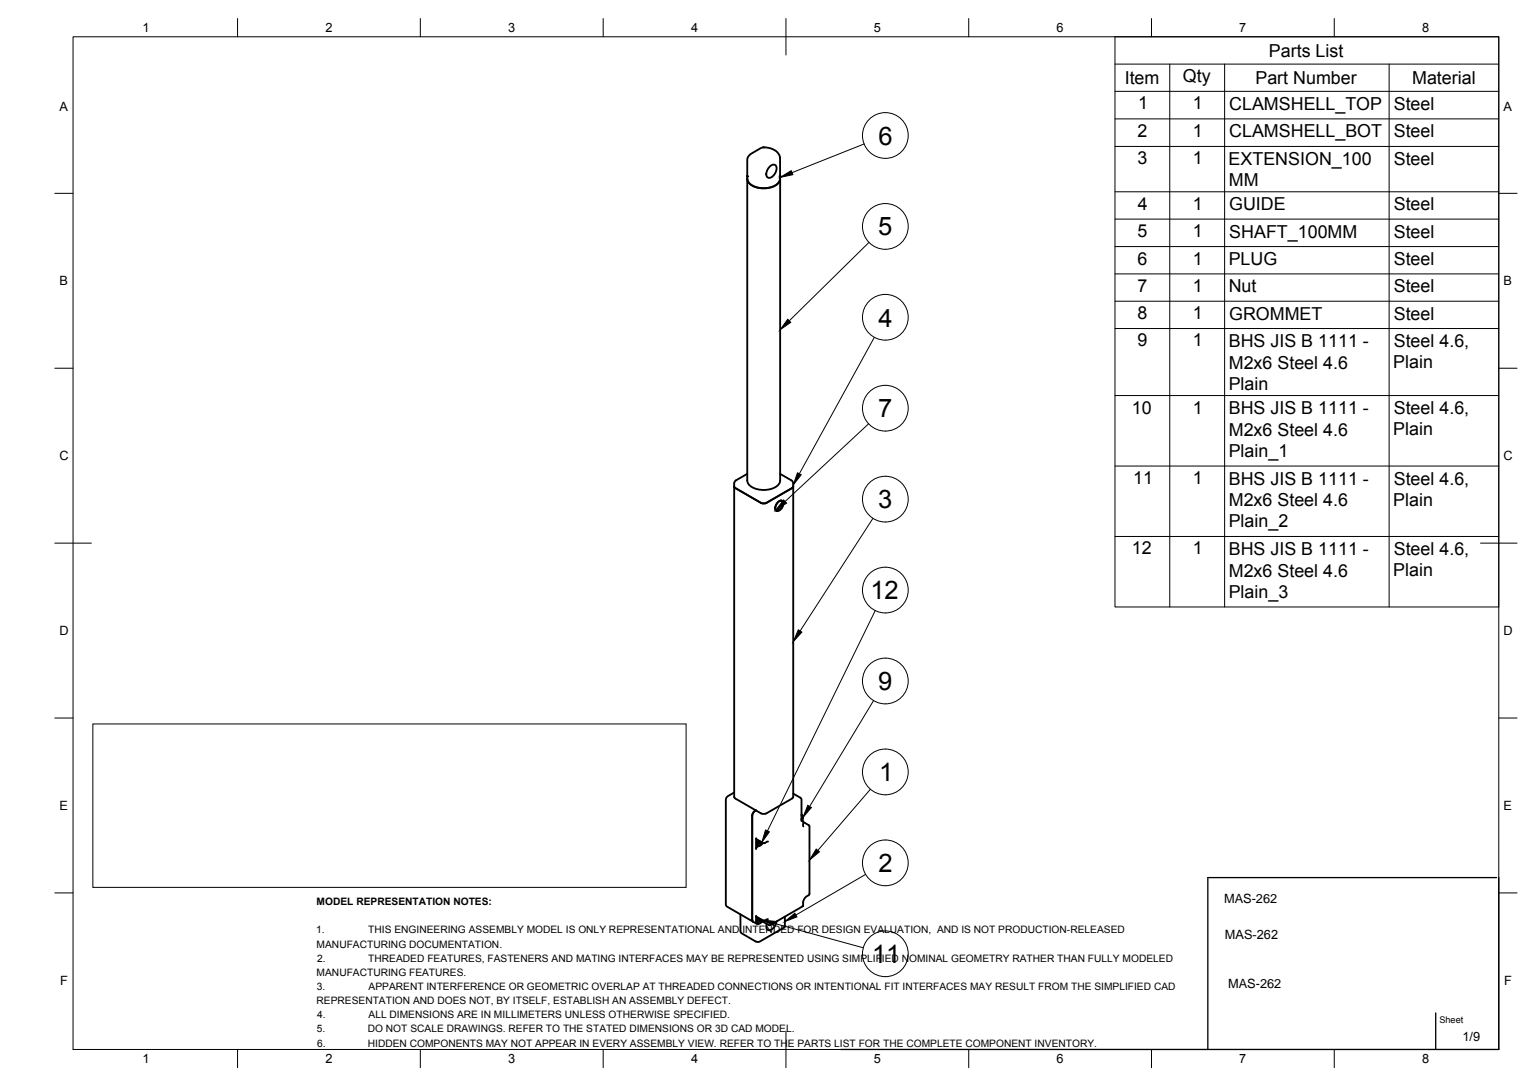
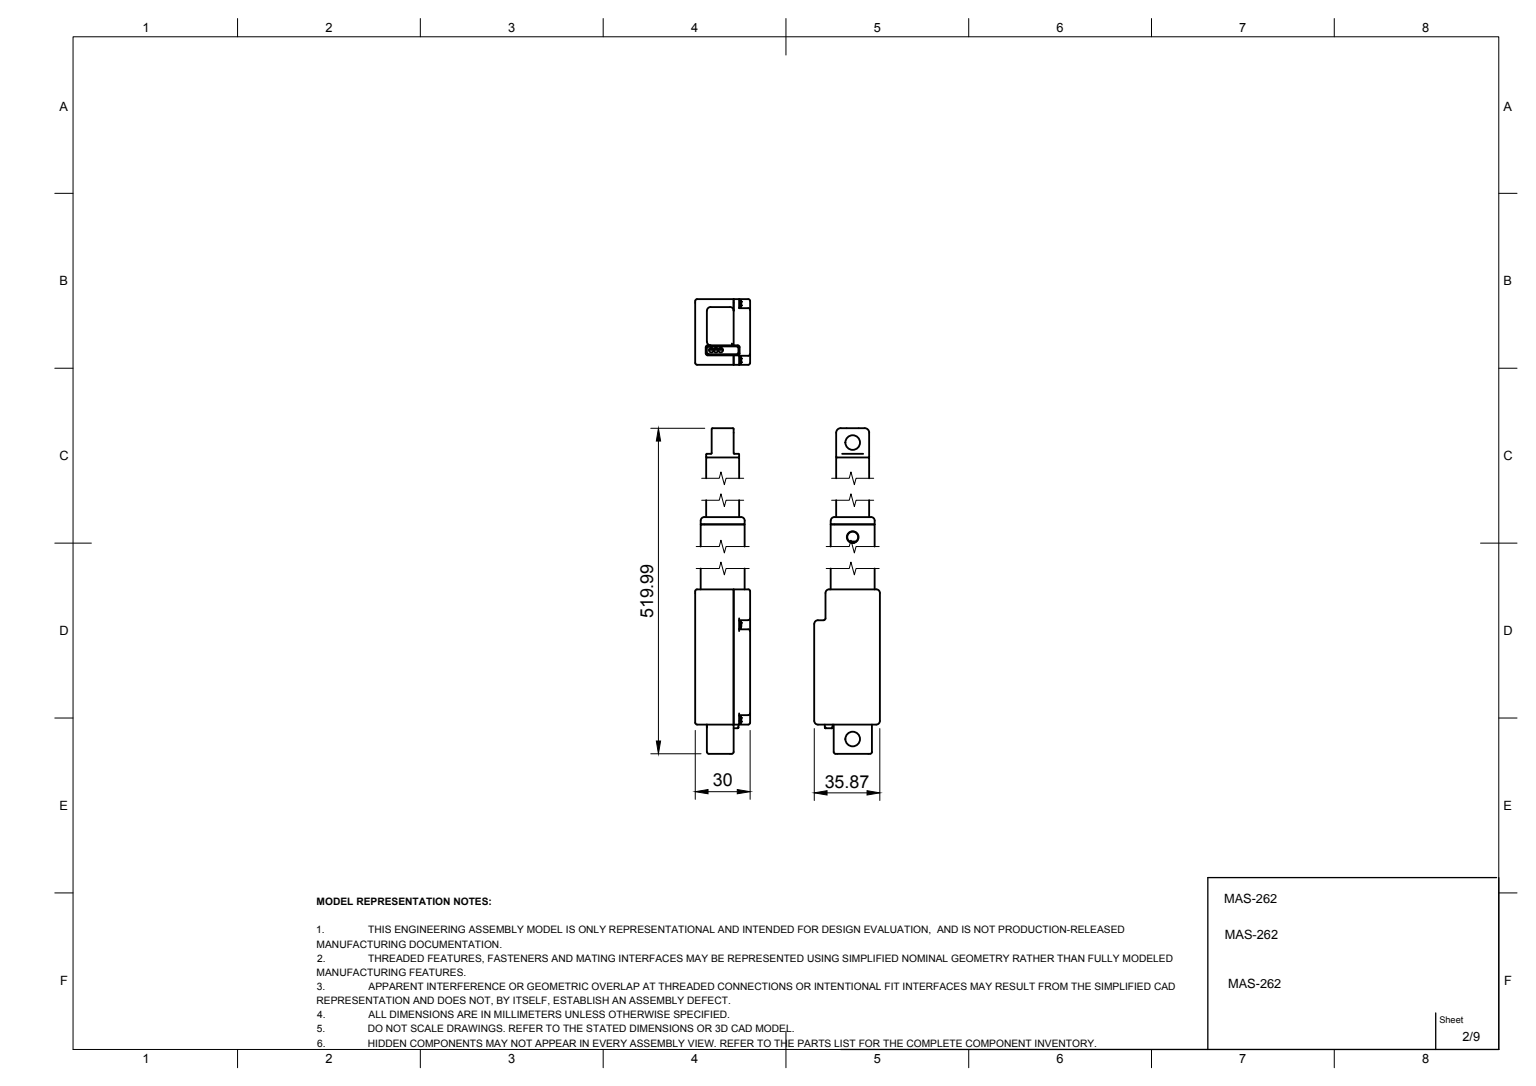
ISO-10303-21;
HEADER;
/* Generated by software containing ST-Developer
 * from STEP Tools, Inc. (www.steptools.com) 
 */

FILE_DESCRIPTION(
/* description */ (''),
/* implementation_level */ '2;1');

FILE_NAME(
/* name */ 'MAS-262',
/* time_stamp */ '2026-10-07T02:13:48+06:00',
/* author */ (''),
/* organization */ (''),
/* preprocessor_version */ 'ST-DEVELOPER v20.2',
/* originating_system */ 'Autodesk Translation Framework v15.15.0.0',
/* authorisation */ '');

FILE_SCHEMA (('AUTOMOTIVE_DESIGN { 1 0 10303 214 3 1 1 }'));
ENDSEC;

DATA;
#10=MECHANICAL_DESIGN_GEOMETRIC_PRESENTATION_REPRESENTATION('',(#114,#115,
#116,#117,#118,#119,#120,#121,#122,#123,#124,#125),#17042);
#11=ITEM_DEFINED_TRANSFORMATION($,$,#8261,#9239);
#12=ITEM_DEFINED_TRANSFORMATION($,$,#8462,#9240);
#13=ITEM_DEFINED_TRANSFORMATION($,$,#8601,#9241);
#14=ITEM_DEFINED_TRANSFORMATION($,$,#8648,#9242);
#15=ITEM_DEFINED_TRANSFORMATION($,$,#8826,#9243);
#16=ITEM_DEFINED_TRANSFORMATION($,$,#8839,#9244);
#17=ITEM_DEFINED_TRANSFORMATION($,$,#8908,#9245);
#18=ITEM_DEFINED_TRANSFORMATION($,$,#8935,#9246);
#19=ITEM_DEFINED_TRANSFORMATION($,$,#8995,#9247);
#20=ITEM_DEFINED_TRANSFORMATION($,$,#9056,#9248);
#21=ITEM_DEFINED_TRANSFORMATION($,$,#9117,#9249);
#22=ITEM_DEFINED_TRANSFORMATION($,$,#9178,#9250);
#23=(
REPRESENTATION_RELATIONSHIP($,$,#17086,#17085)
REPRESENTATION_RELATIONSHIP_WITH_TRANSFORMATION(#11)
SHAPE_REPRESENTATION_RELATIONSHIP()
);
#24=(
REPRESENTATION_RELATIONSHIP($,$,#17087,#17085)
REPRESENTATION_RELATIONSHIP_WITH_TRANSFORMATION(#12)
SHAPE_REPRESENTATION_RELATIONSHIP()
);
#25=(
REPRESENTATION_RELATIONSHIP($,$,#17088,#17085)
REPRESENTATION_RELATIONSHIP_WITH_TRANSFORMATION(#13)
SHAPE_REPRESENTATION_RELATIONSHIP()
);
#26=(
REPRESENTATION_RELATIONSHIP($,$,#17089,#17085)
REPRESENTATION_RELATIONSHIP_WITH_TRANSFORMATION(#14)
SHAPE_REPRESENTATION_RELATIONSHIP()
);
#27=(
REPRESENTATION_RELATIONSHIP($,$,#17090,#17085)
REPRESENTATION_RELATIONSHIP_WITH_TRANSFORMATION(#15)
SHAPE_REPRESENTATION_RELATIONSHIP()
);
#28=(
REPRESENTATION_RELATIONSHIP($,$,#17091,#17085)
REPRESENTATION_RELATIONSHIP_WITH_TRANSFORMATION(#16)
SHAPE_REPRESENTATION_RELATIONSHIP()
);
#29=(
REPRESENTATION_RELATIONSHIP($,$,#17092,#17085)
REPRESENTATION_RELATIONSHIP_WITH_TRANSFORMATION(#17)
SHAPE_REPRESENTATION_RELATIONSHIP()
);
#30=(
REPRESENTATION_RELATIONSHIP($,$,#17093,#17085)
REPRESENTATION_RELATIONSHIP_WITH_TRANSFORMATION(#18)
SHAPE_REPRESENTATION_RELATIONSHIP()
);
#31=(
REPRESENTATION_RELATIONSHIP($,$,#17094,#17085)
REPRESENTATION_RELATIONSHIP_WITH_TRANSFORMATION(#19)
SHAPE_REPRESENTATION_RELATIONSHIP()
);
#32=(
REPRESENTATION_RELATIONSHIP($,$,#17095,#17085)
REPRESENTATION_RELATIONSHIP_WITH_TRANSFORMATION(#20)
SHAPE_REPRESENTATION_RELATIONSHIP()
);
#33=(
REPRESENTATION_RELATIONSHIP($,$,#17096,#17085)
REPRESENTATION_RELATIONSHIP_WITH_TRANSFORMATION(#21)
SHAPE_REPRESENTATION_RELATIONSHIP()
);
#34=(
REPRESENTATION_RELATIONSHIP($,$,#17097,#17085)
REPRESENTATION_RELATIONSHIP_WITH_TRANSFORMATION(#22)
SHAPE_REPRESENTATION_RELATIONSHIP()
);
#35=CONTEXT_DEPENDENT_SHAPE_REPRESENTATION(#23,#17073);
#36=CONTEXT_DEPENDENT_SHAPE_REPRESENTATION(#24,#17074);
#37=CONTEXT_DEPENDENT_SHAPE_REPRESENTATION(#25,#17075);
#38=CONTEXT_DEPENDENT_SHAPE_REPRESENTATION(#26,#17076);
#39=CONTEXT_DEPENDENT_SHAPE_REPRESENTATION(#27,#17077);
#40=CONTEXT_DEPENDENT_SHAPE_REPRESENTATION(#28,#17078);
#41=CONTEXT_DEPENDENT_SHAPE_REPRESENTATION(#29,#17079);
#42=CONTEXT_DEPENDENT_SHAPE_REPRESENTATION(#30,#17080);
#43=CONTEXT_DEPENDENT_SHAPE_REPRESENTATION(#31,#17081);
#44=CONTEXT_DEPENDENT_SHAPE_REPRESENTATION(#32,#17082);
#45=CONTEXT_DEPENDENT_SHAPE_REPRESENTATION(#33,#17083);
#46=CONTEXT_DEPENDENT_SHAPE_REPRESENTATION(#34,#17084);
#47=NEXT_ASSEMBLY_USAGE_OCCURRENCE('CLAMSHELL_TOP:1','CLAMSHELL_TOP:1',
'CLAMSHELL_TOP:1',#17099,#17100,'CLAMSHELL_TOP:1');
#48=NEXT_ASSEMBLY_USAGE_OCCURRENCE('CLAMSHELL_BOT:1','CLAMSHELL_BOT:1',
'CLAMSHELL_BOT:1',#17099,#17101,'CLAMSHELL_BOT:1');
#49=NEXT_ASSEMBLY_USAGE_OCCURRENCE('EXTENSION_100MM:1',
'EXTENSION_100MM:1','EXTENSION_100MM:1',#17099,#17102,
'EXTENSION_100MM:1');
#50=NEXT_ASSEMBLY_USAGE_OCCURRENCE('GUIDE:1','GUIDE:1','GUIDE:1',#17099,
#17103,'GUIDE:1');
#51=NEXT_ASSEMBLY_USAGE_OCCURRENCE('SHAFT_100MM:1','SHAFT_100MM:1',
'SHAFT_100MM:1',#17099,#17104,'SHAFT_100MM:1');
#52=NEXT_ASSEMBLY_USAGE_OCCURRENCE('PLUG:1','PLUG:1','PLUG:1',#17099,#17105,
'PLUG:1');
#53=NEXT_ASSEMBLY_USAGE_OCCURRENCE('Nut:1','Nut:1','Nut:1',#17099,#17106,
'Nut:1');
#54=NEXT_ASSEMBLY_USAGE_OCCURRENCE('GROMMET:1','GROMMET:1','GROMMET:1',
#17099,#17107,'GROMMET:1');
#55=NEXT_ASSEMBLY_USAGE_OCCURRENCE(
'Binding Head Screw JIS B 1111 - M2x6 Steel 4.6 Plain v1:1',
'Binding Head Screw JIS B 1111 - M2x6 Steel 4.6 Plain v1:1',
'Binding Head Screw JIS B 1111 - M2x6 Steel 4.6 Plain v1:1',#17099,#17108,
'Binding Head Screw JIS B 1111 - M2x6 Steel 4.6 Plain v1:1');
#56=NEXT_ASSEMBLY_USAGE_OCCURRENCE(
'Binding Head Screw JIS B 1111 - M2x6 Steel 4.6 Plain v1 (2):1',
'Binding Head Screw JIS B 1111 - M2x6 Steel 4.6 Plain v1 (2):1',
'Binding Head Screw JIS B 1111 - M2x6 Steel 4.6 Plain v1 (2):1',#17099,
#17109,'Binding Head Screw JIS B 1111 - M2x6 Steel 4.6 Plain v1 (2):1');
#57=NEXT_ASSEMBLY_USAGE_OCCURRENCE(
'Binding Head Screw JIS B 1111 - M2x6 Steel 4.6 Plain v1 (3):1',
'Binding Head Screw JIS B 1111 - M2x6 Steel 4.6 Plain v1 (3):1',
'Binding Head Screw JIS B 1111 - M2x6 Steel 4.6 Plain v1 (3):1',#17099,
#17110,'Binding Head Screw JIS B 1111 - M2x6 Steel 4.6 Plain v1 (3):1');
#58=NEXT_ASSEMBLY_USAGE_OCCURRENCE(
'Binding Head Screw JIS B 1111 - M2x6 Steel 4.6 Plain v1 (1):1',
'Binding Head Screw JIS B 1111 - M2x6 Steel 4.6 Plain v1 (1):1',
'Binding Head Screw JIS B 1111 - M2x6 Steel 4.6 Plain v1 (1):1',#17099,
#17111,'Binding Head Screw JIS B 1111 - M2x6 Steel 4.6 Plain v1 (1):1');
#59=CONICAL_SURFACE('',#8827,7.5,0.785398163397441);
#60=CONICAL_SURFACE('',#8834,7.5,0.785398163397441);
#61=CONICAL_SURFACE('',#8902,5.5,0.785398163397441);
#62=CONICAL_SURFACE('',#9046,0.919615242270664,0.261799387799148);
#63=CONICAL_SURFACE('',#9055,2.11281731799709,0.0872664626099693);
#64=CONICAL_SURFACE('',#9107,0.919615242270664,0.261799387799148);
#65=CONICAL_SURFACE('',#9116,2.11281731799709,0.0872664626099693);
#66=CONICAL_SURFACE('',#9168,0.919615242270664,0.261799387799148);
#67=CONICAL_SURFACE('',#9177,2.11281731799709,0.0872664626099693);
#68=CONICAL_SURFACE('',#9229,0.919615242270664,0.261799387799148);
#69=CONICAL_SURFACE('',#9238,2.11281731799709,0.0872664626099693);
#70=B_SPLINE_SURFACE_WITH_KNOTS('',3,3,((#13032,#13033,#13034,#13035,#13036),
(#13037,#13038,#13039,#13040,#13041),(#13042,#13043,#13044,#13045,#13046),
(#13047,#13048,#13049,#13050,#13051),(#13052,#13053,#13054,#13055,#13056),
(#13057,#13058,#13059,#13060,#13061),(#13062,#13063,#13064,#13065,#13066)),
 .UNSPECIFIED.,.F.,.F.,.F.,(4,1,1,1,4),(4,1,4),(0.,0.285714285714286,0.571428571428571,
0.857142857142857,1.),(0.,0.020779022277979,0.0415580445559579),
 .UNSPECIFIED.);
#71=B_SPLINE_SURFACE_WITH_KNOTS('',3,3,((#13080,#13081,#13082,#13083,#13084,
#13085),(#13086,#13087,#13088,#13089,#13090,#13091),(#13092,#13093,#13094,
#13095,#13096,#13097),(#13098,#13099,#13100,#13101,#13102,#13103),(#13104,
#13105,#13106,#13107,#13108,#13109),(#13110,#13111,#13112,#13113,#13114,
#13115),(#13116,#13117,#13118,#13119,#13120,#13121)),.UNSPECIFIED.,.F.,
 .F.,.F.,(4,1,1,1,4),(4,1,1,4),(0.,0.285714285714286,0.571428571428571,
0.857142857142857,1.),(-0.417579612421967,-0.0596542303459957,0.178962691037985,
0.417579612421966),.UNSPECIFIED.);
#72=B_SPLINE_SURFACE_WITH_KNOTS('',3,3,((#13127,#13128,#13129,#13130,#13131),
(#13132,#13133,#13134,#13135,#13136),(#13137,#13138,#13139,#13140,#13141),
(#13142,#13143,#13144,#13145,#13146),(#13147,#13148,#13149,#13150,#13151),
(#13152,#13153,#13154,#13155,#13156),(#13157,#13158,#13159,#13160,#13161)),
 .UNSPECIFIED.,.F.,.F.,.F.,(4,1,1,1,4),(4,1,4),(0.,0.285714285714286,0.571428571428571,
0.857142857142857,1.),(0.,0.0207805027277528,0.0415610054555056),
 .UNSPECIFIED.);
#73=B_SPLINE_SURFACE_WITH_KNOTS('',3,3,((#13236,#13237,#13238,#13239,#13240),
(#13241,#13242,#13243,#13244,#13245),(#13246,#13247,#13248,#13249,#13250),
(#13251,#13252,#13253,#13254,#13255),(#13256,#13257,#13258,#13259,#13260),
(#13261,#13262,#13263,#13264,#13265),(#13266,#13267,#13268,#13269,#13270)),
 .UNSPECIFIED.,.F.,.F.,.F.,(4,1,1,1,4),(4,1,4),(0.,0.285714285714286,0.571428571428571,
0.857142857142857,1.),(0.,0.0207790222779789,0.0415580445559579),
 .UNSPECIFIED.);
#74=B_SPLINE_SURFACE_WITH_KNOTS('',3,3,((#13284,#13285,#13286,#13287,#13288,
#13289),(#13290,#13291,#13292,#13293,#13294,#13295),(#13296,#13297,#13298,
#13299,#13300,#13301),(#13302,#13303,#13304,#13305,#13306,#13307),(#13308,
#13309,#13310,#13311,#13312,#13313),(#13314,#13315,#13316,#13317,#13318,
#13319),(#13320,#13321,#13322,#13323,#13324,#13325)),.UNSPECIFIED.,.F.,
 .F.,.F.,(4,1,1,1,4),(4,1,1,4),(0.,0.285714285714286,0.571428571428571,
0.857142857142857,1.),(-0.417579612421968,-0.0596542303459959,0.178962691037985,
0.417579612421966),.UNSPECIFIED.);
#75=B_SPLINE_SURFACE_WITH_KNOTS('',3,3,((#13331,#13332,#13333,#13334,#13335),
(#13336,#13337,#13338,#13339,#13340),(#13341,#13342,#13343,#13344,#13345),
(#13346,#13347,#13348,#13349,#13350),(#13351,#13352,#13353,#13354,#13355),
(#13356,#13357,#13358,#13359,#13360),(#13361,#13362,#13363,#13364,#13365)),
 .UNSPECIFIED.,.F.,.F.,.F.,(4,1,1,1,4),(4,1,4),(0.,0.285714285714286,0.571428571428571,
0.857142857142857,1.),(0.,0.0207805027277526,0.0415610054555052),
 .UNSPECIFIED.);
#76=B_SPLINE_SURFACE_WITH_KNOTS('',3,3,((#13698,#13699,#13700,#13701,#13702,
#13703),(#13704,#13705,#13706,#13707,#13708,#13709),(#13710,#13711,#13712,
#13713,#13714,#13715),(#13716,#13717,#13718,#13719,#13720,#13721),(#13722,
#13723,#13724,#13725,#13726,#13727)),.UNSPECIFIED.,.F.,.F.,.F.,(4,1,4),
(4,1,1,4),(0.,0.5,1.),(0.,0.0435664957825988,0.0599039317010734,0.0762413676195479),
 .UNSPECIFIED.);
#77=B_SPLINE_SURFACE_WITH_KNOTS('',3,3,((#13746,#13747,#13748,#13749,#13750,
#13751),(#13752,#13753,#13754,#13755,#13756,#13757),(#13758,#13759,#13760,
#13761,#13762,#13763),(#13764,#13765,#13766,#13767,#13768,#13769),(#13770,
#13771,#13772,#13773,#13774,#13775)),.UNSPECIFIED.,.F.,.F.,.F.,(4,1,4),
(4,1,1,4),(0.,0.5,1.),(0.,0.0163372895861103,0.0326745791722206,0.0762406847351813),
 .UNSPECIFIED.);
#78=B_SPLINE_SURFACE_WITH_KNOTS('',3,3,((#13800,#13801,#13802,#13803,#13804,
#13805),(#13806,#13807,#13808,#13809,#13810,#13811),(#13812,#13813,#13814,
#13815,#13816,#13817),(#13818,#13819,#13820,#13821,#13822,#13823),(#13824,
#13825,#13826,#13827,#13828,#13829)),.UNSPECIFIED.,.F.,.F.,.F.,(4,1,4),
(4,1,1,4),(0.,0.5,1.),(3.96177645312185E-16,0.061147749085529,0.0917216236282934,
0.214017121799351),.UNSPECIFIED.);
#79=B_SPLINE_SURFACE_WITH_KNOTS('',3,3,((#13851,#13852,#13853,#13854,#13855,
#13856),(#13857,#13858,#13859,#13860,#13861,#13862),(#13863,#13864,#13865,
#13866,#13867,#13868),(#13869,#13870,#13871,#13872,#13873,#13874),(#13875,
#13876,#13877,#13878,#13879,#13880)),.UNSPECIFIED.,.F.,.F.,.F.,(4,1,4),
(4,1,1,4),(0.,0.5,1.),(2.01858731750029E-18,0.0917257862177262,0.152876310362877,
0.214026834508028),.UNSPECIFIED.);
#80=B_SPLINE_SURFACE_WITH_KNOTS('',3,3,((#13926,#13927,#13928,#13929,#13930,
#13931),(#13932,#13933,#13934,#13935,#13936,#13937),(#13938,#13939,#13940,
#13941,#13942,#13943),(#13944,#13945,#13946,#13947,#13948,#13949),(#13950,
#13951,#13952,#13953,#13954,#13955)),.UNSPECIFIED.,.F.,.F.,.F.,(4,1,4),
(4,1,1,4),(0.,0.5,1.),(0.,0.0163372896496662,0.0326745792993324,0.0762406850317755),
 .UNSPECIFIED.);
#81=B_SPLINE_SURFACE_WITH_KNOTS('',3,3,((#13974,#13975,#13976,#13977,#13978,
#13979),(#13980,#13981,#13982,#13983,#13984,#13985),(#13986,#13987,#13988,
#13989,#13990,#13991),(#13992,#13993,#13994,#13995,#13996,#13997),(#13998,
#13999,#14000,#14001,#14002,#14003)),.UNSPECIFIED.,.F.,.F.,.F.,(4,1,4),
(4,1,1,4),(0.,0.5,1.),(7.01665201425609E-18,0.0435664948259872,0.0599039303857324,
0.0762413659454776),.UNSPECIFIED.);
#82=B_SPLINE_SURFACE_WITH_KNOTS('',3,3,((#14027,#14028,#14029,#14030,#14031,
#14032),(#14033,#14034,#14035,#14036,#14037,#14038),(#14039,#14040,#14041,
#14042,#14043,#14044),(#14045,#14046,#14047,#14048,#14049,#14050),(#14051,
#14052,#14053,#14054,#14055,#14056)),.UNSPECIFIED.,.F.,.F.,.F.,(4,1,4),
(4,1,1,4),(0.,0.5,1.),(6.74145042959343E-15,0.0611477488274177,0.0917216232411232,
0.214017120895945),.UNSPECIFIED.);
#83=B_SPLINE_SURFACE_WITH_KNOTS('',3,3,((#14069,#14070,#14071,#14072,#14073,
#14074),(#14075,#14076,#14077,#14078,#14079,#14080),(#14081,#14082,#14083,
#14084,#14085,#14086),(#14087,#14088,#14089,#14090,#14091,#14092),(#14093,
#14094,#14095,#14096,#14097,#14098)),.UNSPECIFIED.,.F.,.F.,.F.,(4,1,4),
(4,1,1,4),(0.,0.5,1.),(0.,0.0917257862177262,0.152876310362877,0.214026834508028),
 .UNSPECIFIED.);
#84=B_SPLINE_SURFACE_WITH_KNOTS('',3,3,((#14832,#14833,#14834,#14835,#14836,
#14837,#14838,#14839,#14840,#14841,#14842,#14843,#14844,#14845,#14846,#14847,
#14848,#14849,#14850,#14851,#14852,#14853,#14854,#14855,#14856,#14857,#14858,
#14859,#14860,#14861,#14862,#14863,#14864,#14865,#14866,#14867,#14868,#14869,
#14870,#14871,#14872,#14873,#14874,#14875,#14876,#14877,#14878,#14879,#14880,
#14881,#14882,#14883,#14884,#14885,#14886,#14887,#14888,#14889,#14890,#14891,
#14892,#14893,#14894,#14895,#14896,#14897,#14898,#14899,#14900,#14901,#14902,
#14903,#14904,#14905,#14906,#14907,#14908,#14909,#14910),(#14911,#14912,
#14913,#14914,#14915,#14916,#14917,#14918,#14919,#14920,#14921,#14922,#14923,
#14924,#14925,#14926,#14927,#14928,#14929,#14930,#14931,#14932,#14933,#14934,
#14935,#14936,#14937,#14938,#14939,#14940,#14941,#14942,#14943,#14944,#14945,
#14946,#14947,#14948,#14949,#14950,#14951,#14952,#14953,#14954,#14955,#14956,
#14957,#14958,#14959,#14960,#14961,#14962,#14963,#14964,#14965,#14966,#14967,
#14968,#14969,#14970,#14971,#14972,#14973,#14974,#14975,#14976,#14977,#14978,
#14979,#14980,#14981,#14982,#14983,#14984,#14985,#14986,#14987,#14988,#14989),
(#14990,#14991,#14992,#14993,#14994,#14995,#14996,#14997,#14998,#14999,
#15000,#15001,#15002,#15003,#15004,#15005,#15006,#15007,#15008,#15009,#15010,
#15011,#15012,#15013,#15014,#15015,#15016,#15017,#15018,#15019,#15020,#15021,
#15022,#15023,#15024,#15025,#15026,#15027,#15028,#15029,#15030,#15031,#15032,
#15033,#15034,#15035,#15036,#15037,#15038,#15039,#15040,#15041,#15042,#15043,
#15044,#15045,#15046,#15047,#15048,#15049,#15050,#15051,#15052,#15053,#15054,
#15055,#15056,#15057,#15058,#15059,#15060,#15061,#15062,#15063,#15064,#15065,
#15066,#15067,#15068),(#15069,#15070,#15071,#15072,#15073,#15074,#15075,
#15076,#15077,#15078,#15079,#15080,#15081,#15082,#15083,#15084,#15085,#15086,
#15087,#15088,#15089,#15090,#15091,#15092,#15093,#15094,#15095,#15096,#15097,
#15098,#15099,#15100,#15101,#15102,#15103,#15104,#15105,#15106,#15107,#15108,
#15109,#15110,#15111,#15112,#15113,#15114,#15115,#15116,#15117,#15118,#15119,
#15120,#15121,#15122,#15123,#15124,#15125,#15126,#15127,#15128,#15129,#15130,
#15131,#15132,#15133,#15134,#15135,#15136,#15137,#15138,#15139,#15140,#15141,
#15142,#15143,#15144,#15145,#15146,#15147)),.UNSPECIFIED.,.F.,.F.,.F.,(4,
4),(4,1,1,1,1,1,1,1,1,1,1,1,1,1,1,1,1,1,1,1,1,1,1,1,1,1,1,1,1,1,1,1,1,1,
1,1,1,1,1,1,1,1,1,1,1,1,1,1,1,1,1,1,1,1,1,1,1,1,1,1,1,1,1,1,1,1,1,1,1,1,
1,1,1,1,1,1,4),(0.,0.0820126057383859),(8.31487785380719,8.80497047640879,
9.29506309901039,9.78515572161199,10.2752483442136,10.7653409668152,11.2554335894168,
11.7455262120184,12.23561883462,12.7257114572216,13.2158040798232,13.7058967024248,
14.1959893250264,14.686081947628,15.1761745702296,15.6662671928312,16.1563598154328,
16.6464524380344,17.136545060636,17.6266376832376,18.1167303058392,18.6068229284408,
19.0969155510424,19.587008173644,20.0771007962456,20.5671934188472,21.0572860414487,
21.5473786640503,22.0374712866519,22.5275639092535,23.0176565318551,23.5077491544567,
23.9978417770583,24.4879343996599,24.9780270222615,25.4681196448631,25.9582122674647,
26.4483048900663,26.9383975126679,27.4284901352695,27.9185827578711,28.4086753804727,
28.8987680030743,29.3888606256759,29.8789532482775,30.3690458708791,30.8591384934807,
31.3492311160823,31.8393237386839,32.3294163612855,32.8195089838871,33.3096016064887,
33.7996942290903,34.2897868516919,34.7798794742935,35.2699720968951,35.7600647194967,
36.2501573420983,36.7402499646999,37.2303425873015,37.7204352099031,38.2105278325047,
38.7006204551063,39.1907130777079,39.6808057003095,40.1708983229111,40.6609909455127,
41.1510835681143,41.6411761907159,42.1312688133175,42.6213614359191,43.1114540585207,
43.6015466811223,44.0916393037239,44.5817319263255,45.0718245489271,45.5619171715287),
 .UNSPECIFIED.);
#85=B_SPLINE_SURFACE_WITH_KNOTS('',3,3,((#15435,#15436,#15437,#15438,#15439,
#15440,#15441,#15442,#15443,#15444,#15445,#15446,#15447,#15448,#15449,#15450,
#15451,#15452,#15453,#15454,#15455,#15456,#15457,#15458,#15459,#15460,#15461,
#15462,#15463,#15464,#15465,#15466,#15467,#15468,#15469,#15470,#15471,#15472,
#15473,#15474,#15475,#15476,#15477,#15478,#15479,#15480,#15481,#15482,#15483,
#15484,#15485,#15486,#15487,#15488,#15489,#15490,#15491,#15492,#15493,#15494,
#15495,#15496,#15497,#15498,#15499,#15500,#15501,#15502,#15503,#15504,#15505,
#15506,#15507,#15508,#15509,#15510,#15511,#15512,#15513),(#15514,#15515,
#15516,#15517,#15518,#15519,#15520,#15521,#15522,#15523,#15524,#15525,#15526,
#15527,#15528,#15529,#15530,#15531,#15532,#15533,#15534,#15535,#15536,#15537,
#15538,#15539,#15540,#15541,#15542,#15543,#15544,#15545,#15546,#15547,#15548,
#15549,#15550,#15551,#15552,#15553,#15554,#15555,#15556,#15557,#15558,#15559,
#15560,#15561,#15562,#15563,#15564,#15565,#15566,#15567,#15568,#15569,#15570,
#15571,#15572,#15573,#15574,#15575,#15576,#15577,#15578,#15579,#15580,#15581,
#15582,#15583,#15584,#15585,#15586,#15587,#15588,#15589,#15590,#15591,#15592),
(#15593,#15594,#15595,#15596,#15597,#15598,#15599,#15600,#15601,#15602,
#15603,#15604,#15605,#15606,#15607,#15608,#15609,#15610,#15611,#15612,#15613,
#15614,#15615,#15616,#15617,#15618,#15619,#15620,#15621,#15622,#15623,#15624,
#15625,#15626,#15627,#15628,#15629,#15630,#15631,#15632,#15633,#15634,#15635,
#15636,#15637,#15638,#15639,#15640,#15641,#15642,#15643,#15644,#15645,#15646,
#15647,#15648,#15649,#15650,#15651,#15652,#15653,#15654,#15655,#15656,#15657,
#15658,#15659,#15660,#15661,#15662,#15663,#15664,#15665,#15666,#15667,#15668,
#15669,#15670,#15671),(#15672,#15673,#15674,#15675,#15676,#15677,#15678,
#15679,#15680,#15681,#15682,#15683,#15684,#15685,#15686,#15687,#15688,#15689,
#15690,#15691,#15692,#15693,#15694,#15695,#15696,#15697,#15698,#15699,#15700,
#15701,#15702,#15703,#15704,#15705,#15706,#15707,#15708,#15709,#15710,#15711,
#15712,#15713,#15714,#15715,#15716,#15717,#15718,#15719,#15720,#15721,#15722,
#15723,#15724,#15725,#15726,#15727,#15728,#15729,#15730,#15731,#15732,#15733,
#15734,#15735,#15736,#15737,#15738,#15739,#15740,#15741,#15742,#15743,#15744,
#15745,#15746,#15747,#15748,#15749,#15750)),.UNSPECIFIED.,.F.,.F.,.F.,(4,
4),(4,1,1,1,1,1,1,1,1,1,1,1,1,1,1,1,1,1,1,1,1,1,1,1,1,1,1,1,1,1,1,1,1,1,
1,1,1,1,1,1,1,1,1,1,1,1,1,1,1,1,1,1,1,1,1,1,1,1,1,1,1,1,1,1,1,1,1,1,1,1,
1,1,1,1,1,1,4),(0.,0.0820126057383859),(11.6150691238056,12.1051617464072,
12.5952543690088,13.0853469916104,13.575439614212,14.0655322368136,14.5556248594152,
15.0457174820168,15.5358101046184,16.02590272722,16.5159953498216,17.0060879724232,
17.4961805950248,17.9862732176264,18.476365840228,18.9664584628296,19.4565510854312,
19.9466437080328,20.4367363306344,20.926828953236,21.4169215758376,21.9070141984391,
22.3971068210408,22.8871994436423,23.3772920662439,23.8673846888455,24.3574773114471,
24.8475699340487,25.3376625566503,25.8277551792519,26.3178478018535,26.8079404244551,
27.2980330470567,27.7881256696583,28.2782182922599,28.7683109148615,29.2584035374631,
29.7484961600647,30.2385887826663,30.7286814052679,31.2187740278695,31.7088666504711,
32.1989592730727,32.6890518956743,33.1791445182759,33.6692371408775,34.1593297634791,
34.6494223860807,35.1395150086823,35.6296076312839,36.1197002538855,36.6097928764871,
37.0998854990887,37.5899781216903,38.0800707442919,38.5701633668935,39.0602559894951,
39.5503486120967,40.0404412346983,40.5305338572999,41.0206264799015,41.5107191025031,
42.0008117251047,42.4909043477063,42.9809969703079,43.4710895929095,43.9611822155111,
44.4512748381127,44.9413674607143,45.4314600833159,45.9215527059175,46.4116453285191,
46.9017379511207,47.3918305737223,47.8819231963239,48.3720158189255,48.8621084415271),
 .UNSPECIFIED.);
#86=B_SPLINE_SURFACE_WITH_KNOTS('',3,3,((#16016,#16017,#16018,#16019,#16020),
(#16021,#16022,#16023,#16024,#16025),(#16026,#16027,#16028,#16029,#16030),
(#16031,#16032,#16033,#16034,#16035),(#16036,#16037,#16038,#16039,#16040)),
 .UNSPECIFIED.,.F.,.F.,.F.,(4,1,4),(4,1,4),(0.,0.5,1.),(0.,0.673198425769241,
1.5707963267949),.UNSPECIFIED.);
#87=B_SPLINE_SURFACE_WITH_KNOTS('',3,3,((#16047,#16048,#16049,#16050,#16051),
(#16052,#16053,#16054,#16055,#16056),(#16057,#16058,#16059,#16060,#16061),
(#16062,#16063,#16064,#16065,#16066),(#16067,#16068,#16069,#16070,#16071)),
 .UNSPECIFIED.,.F.,.F.,.F.,(4,1,4),(4,1,4),(0.,0.5,1.),(1.73472347597681E-16,
0.673198425769242,1.5707963267949),.UNSPECIFIED.);
#88=B_SPLINE_SURFACE_WITH_KNOTS('',3,3,((#16078,#16079,#16080,#16081,#16082),
(#16083,#16084,#16085,#16086,#16087),(#16088,#16089,#16090,#16091,#16092),
(#16093,#16094,#16095,#16096,#16097),(#16098,#16099,#16100,#16101,#16102)),
 .UNSPECIFIED.,.F.,.F.,.F.,(4,1,4),(4,1,4),(0.,0.5,1.),(0.,0.673198425769241,
1.5707963267949),.UNSPECIFIED.);
#89=B_SPLINE_SURFACE_WITH_KNOTS('',3,3,((#16109,#16110,#16111,#16112,#16113),
(#16114,#16115,#16116,#16117,#16118),(#16119,#16120,#16121,#16122,#16123),
(#16124,#16125,#16126,#16127,#16128),(#16129,#16130,#16131,#16132,#16133)),
 .UNSPECIFIED.,.F.,.F.,.F.,(4,1,4),(4,1,4),(0.,0.5,1.),(0.,0.673198425769241,
1.5707963267949),.UNSPECIFIED.);
#90=SHAPE_REPRESENTATION_RELATIONSHIP('SRR','None',#17086,#102);
#91=SHAPE_REPRESENTATION_RELATIONSHIP('SRR','None',#17087,#103);
#92=SHAPE_REPRESENTATION_RELATIONSHIP('SRR','None',#17088,#104);
#93=SHAPE_REPRESENTATION_RELATIONSHIP('SRR','None',#17089,#105);
#94=SHAPE_REPRESENTATION_RELATIONSHIP('SRR','None',#17090,#106);
#95=SHAPE_REPRESENTATION_RELATIONSHIP('SRR','None',#17091,#107);
#96=SHAPE_REPRESENTATION_RELATIONSHIP('SRR','None',#17092,#108);
#97=SHAPE_REPRESENTATION_RELATIONSHIP('SRR','None',#17093,#109);
#98=SHAPE_REPRESENTATION_RELATIONSHIP('SRR','None',#17094,#110);
#99=SHAPE_REPRESENTATION_RELATIONSHIP('SRR','None',#17095,#111);
#100=SHAPE_REPRESENTATION_RELATIONSHIP('SRR','None',#17096,#112);
#101=SHAPE_REPRESENTATION_RELATIONSHIP('SRR','None',#17097,#113);
#102=ADVANCED_BREP_SHAPE_REPRESENTATION('',(#126),#17030);
#103=ADVANCED_BREP_SHAPE_REPRESENTATION('',(#127),#17031);
#104=ADVANCED_BREP_SHAPE_REPRESENTATION('',(#128),#17032);
#105=ADVANCED_BREP_SHAPE_REPRESENTATION('',(#129),#17033);
#106=ADVANCED_BREP_SHAPE_REPRESENTATION('',(#130),#17034);
#107=ADVANCED_BREP_SHAPE_REPRESENTATION('',(#131),#17035);
#108=ADVANCED_BREP_SHAPE_REPRESENTATION('',(#132),#17036);
#109=ADVANCED_BREP_SHAPE_REPRESENTATION('',(#133),#17037);
#110=ADVANCED_BREP_SHAPE_REPRESENTATION('',(#134),#17038);
#111=ADVANCED_BREP_SHAPE_REPRESENTATION('',(#135),#17039);
#112=ADVANCED_BREP_SHAPE_REPRESENTATION('',(#136),#17040);
#113=ADVANCED_BREP_SHAPE_REPRESENTATION('',(#137),#17041);
#114=STYLED_ITEM('',(#17154),#126);
#115=STYLED_ITEM('',(#17154),#127);
#116=STYLED_ITEM('',(#17154),#128);
#117=STYLED_ITEM('',(#17154),#129);
#118=STYLED_ITEM('',(#17154),#130);
#119=STYLED_ITEM('',(#17154),#131);
#120=STYLED_ITEM('',(#17154),#132);
#121=STYLED_ITEM('',(#17154),#133);
#122=STYLED_ITEM('',(#17154),#134);
#123=STYLED_ITEM('',(#17154),#135);
#124=STYLED_ITEM('',(#17154),#136);
#125=STYLED_ITEM('',(#17154),#137);
#126=MANIFOLD_SOLID_BREP('Body1',#8115);
#127=MANIFOLD_SOLID_BREP('Body1',#8116);
#128=MANIFOLD_SOLID_BREP('Body1',#8117);
#129=MANIFOLD_SOLID_BREP('Body1',#8118);
#130=MANIFOLD_SOLID_BREP('Body1',#8119);
#131=MANIFOLD_SOLID_BREP('Body1',#8120);
#132=MANIFOLD_SOLID_BREP('Body1',#8121);
#133=MANIFOLD_SOLID_BREP('Body1',#8122);
#134=MANIFOLD_SOLID_BREP('Body1',#8123);
#135=MANIFOLD_SOLID_BREP('Body1',#8124);
#136=MANIFOLD_SOLID_BREP('Body1',#8125);
#137=MANIFOLD_SOLID_BREP('Body1',#8126);
#138=FACE_BOUND('',#1043,.T.);
#139=FACE_BOUND('',#1045,.T.);
#140=FACE_BOUND('',#1050,.T.);
#141=FACE_BOUND('',#1052,.T.);
#142=FACE_BOUND('',#1059,.T.);
#143=FACE_BOUND('',#1060,.T.);
#144=FACE_BOUND('',#1071,.T.);
#145=FACE_BOUND('',#1079,.T.);
#146=FACE_BOUND('',#1085,.T.);
#147=FACE_BOUND('',#1086,.T.);
#148=FACE_BOUND('',#1141,.T.);
#149=FACE_BOUND('',#1145,.T.);
#150=FACE_BOUND('',#1146,.T.);
#151=FACE_BOUND('',#1151,.T.);
#152=FACE_BOUND('',#1152,.T.);
#153=FACE_BOUND('',#1157,.T.);
#154=FACE_BOUND('',#1158,.T.);
#155=FACE_BOUND('',#1163,.T.);
#156=FACE_BOUND('',#1164,.T.);
#157=FACE_BOUND('',#1167,.T.);
#158=FACE_BOUND('',#1181,.T.);
#159=FACE_BOUND('',#1228,.T.);
#160=FACE_BOUND('',#1237,.T.);
#161=FACE_BOUND('',#1260,.T.);
#162=FACE_BOUND('',#1264,.T.);
#163=FACE_BOUND('',#1267,.T.);
#164=FACE_BOUND('',#1281,.T.);
#165=FACE_BOUND('',#1294,.T.);
#166=FACE_BOUND('',#1299,.T.);
#167=FACE_BOUND('',#1304,.T.);
#168=FACE_BOUND('',#1324,.T.);
#169=FACE_BOUND('',#1327,.T.);
#170=FACE_BOUND('',#1329,.T.);
#171=FACE_BOUND('',#1345,.T.);
#172=FACE_BOUND('',#1355,.T.);
#173=FACE_BOUND('',#1357,.T.);
#174=FACE_BOUND('',#1385,.T.);
#175=FACE_BOUND('',#1411,.T.);
#176=FACE_BOUND('',#1437,.T.);
#177=FACE_BOUND('',#1463,.T.);
#178=(
BOUNDED_SURFACE()
B_SPLINE_SURFACE(2,2,((#12260,#12261,#12262),(#12263,#12264,#12265),(#12266,
#12267,#12268)),.UNSPECIFIED.,.F.,.F.,.F.)
B_SPLINE_SURFACE_WITH_KNOTS((3,3),(3,3),(-1.5707963267949,0.),(0.,1.5707963267949),
 .UNSPECIFIED.)
GEOMETRIC_REPRESENTATION_ITEM()
RATIONAL_B_SPLINE_SURFACE(((1.,0.707106781186548,1.),(0.707106781186558,
0.500000000000007,0.707106781186558),(1.,0.707106781186548,1.)))
REPRESENTATION_ITEM('')
SURFACE()
);
#179=(
BOUNDED_SURFACE()
B_SPLINE_SURFACE(2,2,((#12273,#12274,#12275),(#12276,#12277,#12278),(#12279,
#12280,#12281)),.UNSPECIFIED.,.F.,.F.,.F.)
B_SPLINE_SURFACE_WITH_KNOTS((3,3),(3,3),(-1.5707963267949,0.),(-1.5707963267949,
0.),.UNSPECIFIED.)
GEOMETRIC_REPRESENTATION_ITEM()
RATIONAL_B_SPLINE_SURFACE(((1.,0.707106781186548,1.),(0.707106781186552,
0.500000000000003,0.707106781186552),(1.,0.707106781186548,1.)))
REPRESENTATION_ITEM('')
SURFACE()
);
#180=(
BOUNDED_SURFACE()
B_SPLINE_SURFACE(2,2,((#12432,#12433,#12434),(#12435,#12436,#12437),(#12438,
#12439,#12440)),.UNSPECIFIED.,.F.,.F.,.F.)
B_SPLINE_SURFACE_WITH_KNOTS((3,3),(3,3),(0.,1.5707963267949),(-1.5707963267949,
0.),.UNSPECIFIED.)
GEOMETRIC_REPRESENTATION_ITEM()
RATIONAL_B_SPLINE_SURFACE(((1.,0.707106781186548,1.),(0.707106781186545,
0.499999999999998,0.707106781186545),(1.,0.707106781186548,1.)))
REPRESENTATION_ITEM('')
SURFACE()
);
#181=(
BOUNDED_SURFACE()
B_SPLINE_SURFACE(2,2,((#12455,#12456,#12457),(#12458,#12459,#12460),(#12461,
#12462,#12463)),.UNSPECIFIED.,.F.,.F.,.F.)
B_SPLINE_SURFACE_WITH_KNOTS((3,3),(3,3),(0.,1.5707963267949),(0.,1.5707963267949),
 .UNSPECIFIED.)
GEOMETRIC_REPRESENTATION_ITEM()
RATIONAL_B_SPLINE_SURFACE(((1.,0.707106781186548,1.),(0.707106781186551,
0.500000000000003,0.707106781186551),(1.,0.707106781186548,1.)))
REPRESENTATION_ITEM('')
SURFACE()
);
#182=(
BOUNDED_SURFACE()
B_SPLINE_SURFACE(2,2,((#12484,#12485,#12486),(#12487,#12488,#12489),(#12490,
#12491,#12492)),.UNSPECIFIED.,.F.,.F.,.F.)
B_SPLINE_SURFACE_WITH_KNOTS((3,3),(3,3),(-1.5707963267949,0.),(-1.5707963267949,
0.),.UNSPECIFIED.)
GEOMETRIC_REPRESENTATION_ITEM()
RATIONAL_B_SPLINE_SURFACE(((1.,0.707106781186548,1.),(0.707106781186551,
0.500000000000002,0.707106781186551),(1.,0.707106781186548,1.)))
REPRESENTATION_ITEM('')
SURFACE()
);
#183=(
BOUNDED_SURFACE()
B_SPLINE_SURFACE(2,2,((#12730,#12731,#12732),(#12733,#12734,#12735),(#12736,
#12737,#12738)),.UNSPECIFIED.,.F.,.F.,.F.)
B_SPLINE_SURFACE_WITH_KNOTS((3,3),(3,3),(0.,1.5707963267949),(-4.44089209850066E-15,
1.57079632679491),.UNSPECIFIED.)
GEOMETRIC_REPRESENTATION_ITEM()
RATIONAL_B_SPLINE_SURFACE(((1.,0.707106781186543,1.),(0.707106781186536,
0.499999999999988,0.707106781186536),(1.,0.707106781186543,1.)))
REPRESENTATION_ITEM('')
SURFACE()
);
#184=(
BOUNDED_SURFACE()
B_SPLINE_SURFACE(2,2,((#12750,#12751,#12752),(#12753,#12754,#12755),(#12756,
#12757,#12758)),.UNSPECIFIED.,.F.,.F.,.F.)
B_SPLINE_SURFACE_WITH_KNOTS((3,3),(3,3),(0.,1.5707963267949),(1.57079632679489,
3.14159265358979),.UNSPECIFIED.)
GEOMETRIC_REPRESENTATION_ITEM()
RATIONAL_B_SPLINE_SURFACE(((1.,0.707106781186546,1.),(0.707106781186536,
0.499999999999991,0.707106781186536),(1.,0.707106781186546,1.)))
REPRESENTATION_ITEM('')
SURFACE()
);
#185=(
BOUNDED_SURFACE()
B_SPLINE_SURFACE(2,2,((#12767,#12768,#12769),(#12770,#12771,#12772),(#12773,
#12774,#12775)),.UNSPECIFIED.,.F.,.F.,.F.)
B_SPLINE_SURFACE_WITH_KNOTS((3,3),(3,3),(0.,1.5707963267949),(-3.14159265358979,
-1.5707963267949),.UNSPECIFIED.)
GEOMETRIC_REPRESENTATION_ITEM()
RATIONAL_B_SPLINE_SURFACE(((1.,0.707106781186547,1.),(0.707106781186536,
0.499999999999992,0.707106781186536),(1.,0.707106781186547,1.)))
REPRESENTATION_ITEM('')
SURFACE()
);
#186=(
BOUNDED_SURFACE()
B_SPLINE_SURFACE(2,2,((#12787,#12788,#12789),(#12790,#12791,#12792),(#12793,
#12794,#12795)),.UNSPECIFIED.,.F.,.F.,.F.)
B_SPLINE_SURFACE_WITH_KNOTS((3,3),(3,3),(0.,1.5707963267949),(-1.5707963267949,
-1.11022302462516E-15),.UNSPECIFIED.)
GEOMETRIC_REPRESENTATION_ITEM()
RATIONAL_B_SPLINE_SURFACE(((1.,0.707106781186548,1.),(0.707106781186552,
0.500000000000004,0.707106781186552),(1.,0.707106781186548,1.)))
REPRESENTATION_ITEM('')
SURFACE()
);
#187=(
BOUNDED_SURFACE()
B_SPLINE_SURFACE(2,2,((#12804,#12805,#12806),(#12807,#12808,#12809),(#12810,
#12811,#12812)),.UNSPECIFIED.,.F.,.F.,.F.)
B_SPLINE_SURFACE_WITH_KNOTS((3,3),(3,3),(0.,1.5707963267949),(1.11022302462515E-15,
1.57079632679489),.UNSPECIFIED.)
GEOMETRIC_REPRESENTATION_ITEM()
RATIONAL_B_SPLINE_SURFACE(((1.,0.707106781186549,1.),(0.707106781186552,
0.500000000000005,0.707106781186552),(1.,0.707106781186549,1.)))
REPRESENTATION_ITEM('')
SURFACE()
);
#188=(
BOUNDED_SURFACE()
B_SPLINE_SURFACE(2,2,((#13423,#13424,#13425),(#13426,#13427,#13428),(#13429,
#13430,#13431)),.UNSPECIFIED.,.F.,.F.,.F.)
B_SPLINE_SURFACE_WITH_KNOTS((3,3),(3,3),(-1.5707963267949,1.77635683940025E-13),
(0.,1.5707963267949),.UNSPECIFIED.)
GEOMETRIC_REPRESENTATION_ITEM()
RATIONAL_B_SPLINE_SURFACE(((1.,0.707106781186548,1.),(0.707106781186393,
0.499999999999891,0.707106781186393),(1.,0.707106781186548,1.)))
REPRESENTATION_ITEM('')
SURFACE()
);
#189=(
BOUNDED_SURFACE()
B_SPLINE_SURFACE(2,2,((#13443,#13444,#13445),(#13446,#13447,#13448),(#13449,
#13450,#13451)),.UNSPECIFIED.,.F.,.F.,.F.)
B_SPLINE_SURFACE_WITH_KNOTS((3,3),(3,3),(-1.5707963267949,0.),(-1.5707963267949,
5.55111512312578E-15),.UNSPECIFIED.)
GEOMETRIC_REPRESENTATION_ITEM()
RATIONAL_B_SPLINE_SURFACE(((1.,0.707106781186546,1.),(0.707106781186793,
0.500000000000172,0.707106781186793),(1.,0.707106781186546,1.)))
REPRESENTATION_ITEM('')
SURFACE()
);
#190=(
BOUNDED_SURFACE()
B_SPLINE_SURFACE(2,2,((#13465,#13466,#13467),(#13468,#13469,#13470),(#13471,
#13472,#13473)),.UNSPECIFIED.,.F.,.F.,.F.)
B_SPLINE_SURFACE_WITH_KNOTS((3,3),(3,3),(-1.5707963267949,0.),(-3.14159265358979,
-1.5707963267949),.UNSPECIFIED.)
GEOMETRIC_REPRESENTATION_ITEM()
RATIONAL_B_SPLINE_SURFACE(((1.,0.707106781186548,1.),(0.707106781186801,
0.50000000000018,0.707106781186801),(1.,0.707106781186548,1.)))
REPRESENTATION_ITEM('')
SURFACE()
);
#191=(
BOUNDED_SURFACE()
B_SPLINE_SURFACE(2,2,((#13485,#13486,#13487),(#13488,#13489,#13490),(#13491,
#13492,#13493)),.UNSPECIFIED.,.F.,.F.,.F.)
B_SPLINE_SURFACE_WITH_KNOTS((3,3),(3,3),(-1.5707963267949,0.),(1.5707963267949,
3.14159265358979),.UNSPECIFIED.)
GEOMETRIC_REPRESENTATION_ITEM()
RATIONAL_B_SPLINE_SURFACE(((1.,0.707106781186547,1.),(0.707106781186801,
0.500000000000179,0.707106781186801),(1.,0.707106781186547,1.)))
REPRESENTATION_ITEM('')
SURFACE()
);
#192=(
BOUNDED_SURFACE()
B_SPLINE_SURFACE(2,2,((#13513,#13514,#13515),(#13516,#13517,#13518),(#13519,
#13520,#13521)),.UNSPECIFIED.,.F.,.F.,.F.)
B_SPLINE_SURFACE_WITH_KNOTS((3,3),(3,3),(-8.32667268468867E-15,1.57079632679493),
(-1.57079632679491,-0.994301061223377),.UNSPECIFIED.)
GEOMETRIC_REPRESENTATION_ITEM()
RATIONAL_B_SPLINE_SURFACE(((1.,0.958743497277462,1.),(0.707106781186526,
0.677934028343379,0.707106781186526),(1.,0.958743497277462,1.)))
REPRESENTATION_ITEM('')
SURFACE()
);
#193=(
BOUNDED_SURFACE()
B_SPLINE_SURFACE(2,2,((#13547,#13548,#13549),(#13550,#13551,#13552),(#13553,
#13554,#13555)),.UNSPECIFIED.,.F.,.F.,.F.)
B_SPLINE_SURFACE_WITH_KNOTS((3,3),(3,3),(0.,1.57079632679491),(0.994301061223376,
1.5707963267949),.UNSPECIFIED.)
GEOMETRIC_REPRESENTATION_ITEM()
RATIONAL_B_SPLINE_SURFACE(((1.,0.958743497277463,1.),(0.707106781186533,
0.677934028343387,0.707106781186533),(1.,0.958743497277463,1.)))
REPRESENTATION_ITEM('')
SURFACE()
);
#194=(
BOUNDED_SURFACE()
B_SPLINE_SURFACE(2,2,((#13571,#13572,#13573),(#13574,#13575,#13576),(#13577,
#13578,#13579)),.UNSPECIFIED.,.F.,.F.,.F.)
B_SPLINE_SURFACE_WITH_KNOTS((3,3),(3,3),(0.,1.57079632679492),(1.5707963267949,
2.14729159236641),.UNSPECIFIED.)
GEOMETRIC_REPRESENTATION_ITEM()
RATIONAL_B_SPLINE_SURFACE(((1.,0.958743497277464,1.),(0.707106781186532,
0.677934028343386,0.707106781186532),(1.,0.958743497277464,1.)))
REPRESENTATION_ITEM('')
SURFACE()
);
#195=(
BOUNDED_SURFACE()
B_SPLINE_SURFACE(2,2,((#13605,#13606,#13607),(#13608,#13609,#13610),(#13611,
#13612,#13613)),.UNSPECIFIED.,.F.,.F.,.F.)
B_SPLINE_SURFACE_WITH_KNOTS((3,3),(3,3),(0.,1.57079632679492),(-2.14729159236642,
-1.57079632679489),.UNSPECIFIED.)
GEOMETRIC_REPRESENTATION_ITEM()
RATIONAL_B_SPLINE_SURFACE(((1.,0.958743497277463,1.),(0.707106781186532,
0.677934028343385,0.707106781186532),(1.,0.958743497277463,1.)))
REPRESENTATION_ITEM('')
SURFACE()
);
#196=SPHERICAL_SURFACE('',#8306,1.);
#197=SPHERICAL_SURFACE('',#8311,1.);
#198=SPHERICAL_SURFACE('',#8414,1.);
#199=SPHERICAL_SURFACE('',#8416,1.);
#200=SPHERICAL_SURFACE('',#8418,1.);
#201=SPHERICAL_SURFACE('',#8420,1.);
#202=SPHERICAL_SURFACE('',#8655,2.);
#203=SPHERICAL_SURFACE('',#8660,2.);
#204=SPHERICAL_SURFACE('',#8665,2.);
#205=SPHERICAL_SURFACE('',#8667,2.);
#206=SPHERICAL_SURFACE('',#8677,0.2);
#207=SPHERICAL_SURFACE('',#8690,0.2);
#208=SPHERICAL_SURFACE('',#8707,0.2);
#209=SPHERICAL_SURFACE('',#8720,0.2);
#210=SPHERICAL_SURFACE('',#9051,6.32965591734106);
#211=SPHERICAL_SURFACE('',#9112,6.32965591734106);
#212=SPHERICAL_SURFACE('',#9173,6.32965591734106);
#213=SPHERICAL_SURFACE('',#9234,6.32965591734106);
#214=TOROIDAL_SURFACE('',#8295,3.5,1.);
#215=TOROIDAL_SURFACE('',#8300,3.5,1.);
#216=TOROIDAL_SURFACE('',#8389,3.5,1.);
#217=TOROIDAL_SURFACE('',#8394,2.,1.);
#218=TOROIDAL_SURFACE('',#8411,3.5,1.);
#219=TOROIDAL_SURFACE('',#8562,2.,1.);
#220=TOROIDAL_SURFACE('',#8702,9.2,0.2);
#221=TOROIDAL_SURFACE('',#8731,9.2,0.2);
#222=TOROIDAL_SURFACE('',#8762,1.39999999999987,0.4);
#223=TOROIDAL_SURFACE('',#8773,1.39999999999987,0.4);
#224=TOROIDAL_SURFACE('',#8782,1.39999999999987,0.4);
#225=TOROIDAL_SURFACE('',#8793,1.39999999999987,0.4);
#226=TOROIDAL_SURFACE('',#8852,8.6,0.4);
#227=TOROIDAL_SURFACE('',#8859,6.5,2.5);
#228=TOROIDAL_SURFACE('',#8875,8.6,0.4);
#229=TOROIDAL_SURFACE('',#8885,6.5,2.5);
#230=TOROIDAL_SURFACE('',#8886,8.6,0.4);
#231=TOROIDAL_SURFACE('',#8891,7.4,0.4);
#232=TOROIDAL_SURFACE('',#8897,6.6,0.4);
#233=TOROIDAL_SURFACE('',#9038,0.939230484541328,0.1);
#234=TOROIDAL_SURFACE('',#9099,0.939230484541328,0.1);
#235=TOROIDAL_SURFACE('',#9160,0.939230484541328,0.1);
#236=TOROIDAL_SURFACE('',#9221,0.939230484541328,0.1);
#237=ELLIPSE('',#8289,1.4142135623731,1.);
#238=ELLIPSE('',#8291,1.41421356237309,1.);
#239=ELLIPSE('',#8484,1.4142135623731,1.);
#240=ELLIPSE('',#8685,16.7697982864697,9.);
#241=ELLIPSE('',#8686,16.8779777985659,9.2);
#242=ELLIPSE('',#8715,16.7697982864697,9.);
#243=ELLIPSE('',#8716,16.8779777985659,9.2);
#244=ELLIPSE('',#8936,0.509901951359279,0.5);
#245=ELLIPSE('',#8937,0.509901951359279,0.5);
#246=ELLIPSE('',#8939,0.509901951359279,0.5);
#247=ELLIPSE('',#8940,0.509901951359279,0.5);
#248=ELLIPSE('',#8942,0.50990195135928,0.5);
#249=ELLIPSE('',#8943,0.509901951359279,0.5);
#250=ELLIPSE('',#8945,0.509901951359279,0.5);
#251=ELLIPSE('',#8946,0.509901951359279,0.5);
#252=ELLIPSE('',#8997,0.992,0.496);
#253=ELLIPSE('',#8999,0.992,0.496);
#254=ELLIPSE('',#9004,0.992,0.496);
#255=ELLIPSE('',#9009,0.992,0.496);
#256=ELLIPSE('',#9014,0.992,0.496);
#257=ELLIPSE('',#9018,0.992,0.496);
#258=ELLIPSE('',#9020,0.992,0.496);
#259=ELLIPSE('',#9025,0.992,0.496);
#260=ELLIPSE('',#9058,0.992,0.496);
#261=ELLIPSE('',#9060,0.992,0.496);
#262=ELLIPSE('',#9065,0.992,0.496);
#263=ELLIPSE('',#9070,0.992,0.496);
#264=ELLIPSE('',#9075,0.992,0.496);
#265=ELLIPSE('',#9079,0.992,0.496);
#266=ELLIPSE('',#9081,0.992,0.496);
#267=ELLIPSE('',#9086,0.992,0.496);
#268=ELLIPSE('',#9119,0.992,0.496);
#269=ELLIPSE('',#9121,0.992,0.496);
#270=ELLIPSE('',#9126,0.992,0.496);
#271=ELLIPSE('',#9131,0.992,0.496);
#272=ELLIPSE('',#9136,0.992,0.496);
#273=ELLIPSE('',#9140,0.992,0.496);
#274=ELLIPSE('',#9142,0.992,0.496);
#275=ELLIPSE('',#9147,0.992,0.496);
#276=ELLIPSE('',#9180,0.992,0.496);
#277=ELLIPSE('',#9182,0.992,0.496);
#278=ELLIPSE('',#9187,0.992,0.496);
#279=ELLIPSE('',#9192,0.992,0.496);
#280=ELLIPSE('',#9197,0.992,0.496);
#281=ELLIPSE('',#9201,0.992,0.496);
#282=ELLIPSE('',#9203,0.992,0.496);
#283=ELLIPSE('',#9208,0.992,0.496);
#284=PLANE('',#8266);
#285=PLANE('',#8267);
#286=PLANE('',#8270);
#287=PLANE('',#8274);
#288=PLANE('',#8275);
#289=PLANE('',#8276);
#290=PLANE('',#8277);
#291=PLANE('',#8313);
#292=PLANE('',#8316);
#293=PLANE('',#8324);
#294=PLANE('',#8325);
#295=PLANE('',#8326);
#296=PLANE('',#8330);
#297=PLANE('',#8334);
#298=PLANE('',#8335);
#299=PLANE('',#8357);
#300=PLANE('',#8358);
#301=PLANE('',#8359);
#302=PLANE('',#8361);
#303=PLANE('',#8362);
#304=PLANE('',#8363);
#305=PLANE('',#8364);
#306=PLANE('',#8365);
#307=PLANE('',#8370);
#308=PLANE('',#8375);
#309=PLANE('',#8376);
#310=PLANE('',#8377);
#311=PLANE('',#8378);
#312=PLANE('',#8380);
#313=PLANE('',#8381);
#314=PLANE('',#8384);
#315=PLANE('',#8385);
#316=PLANE('',#8424);
#317=PLANE('',#8427);
#318=PLANE('',#8432);
#319=PLANE('',#8439);
#320=PLANE('',#8442);
#321=PLANE('',#8443);
#322=PLANE('',#8446);
#323=PLANE('',#8448);
#324=PLANE('',#8450);
#325=PLANE('',#8453);
#326=PLANE('',#8454);
#327=PLANE('',#8456);
#328=PLANE('',#8457);
#329=PLANE('',#8458);
#330=PLANE('',#8463);
#331=PLANE('',#8491);
#332=PLANE('',#8494);
#333=PLANE('',#8496);
#334=PLANE('',#8500);
#335=PLANE('',#8501);
#336=PLANE('',#8506);
#337=PLANE('',#8507);
#338=PLANE('',#8508);
#339=PLANE('',#8513);
#340=PLANE('',#8523);
#341=PLANE('',#8524);
#342=PLANE('',#8528);
#343=PLANE('',#8529);
#344=PLANE('',#8530);
#345=PLANE('',#8531);
#346=PLANE('',#8537);
#347=PLANE('',#8538);
#348=PLANE('',#8539);
#349=PLANE('',#8541);
#350=PLANE('',#8546);
#351=PLANE('',#8549);
#352=PLANE('',#8552);
#353=PLANE('',#8555);
#354=PLANE('',#8558);
#355=PLANE('',#8591);
#356=PLANE('',#8593);
#357=PLANE('',#8595);
#358=PLANE('',#8596);
#359=PLANE('',#8599);
#360=PLANE('',#8614);
#361=PLANE('',#8623);
#362=PLANE('',#8626);
#363=PLANE('',#8629);
#364=PLANE('',#8632);
#365=PLANE('',#8635);
#366=PLANE('',#8638);
#367=PLANE('',#8641);
#368=PLANE('',#8644);
#369=PLANE('',#8647);
#370=PLANE('',#8671);
#371=PLANE('',#8674);
#372=PLANE('',#8675);
#373=PLANE('',#8693);
#374=PLANE('',#8696);
#375=PLANE('',#8699);
#376=PLANE('',#8722);
#377=PLANE('',#8725);
#378=PLANE('',#8728);
#379=PLANE('',#8746);
#380=PLANE('',#8758);
#381=PLANE('',#8769);
#382=PLANE('',#8789);
#383=PLANE('',#8801);
#384=PLANE('',#8802);
#385=PLANE('',#8805);
#386=PLANE('',#8806);
#387=PLANE('',#8807);
#388=PLANE('',#8808);
#389=PLANE('',#8821);
#390=PLANE('',#8824);
#391=PLANE('',#8825);
#392=PLANE('',#8832);
#393=PLANE('',#8836);
#394=PLANE('',#8856);
#395=PLANE('',#8861);
#396=PLANE('',#8863);
#397=PLANE('',#8882);
#398=PLANE('',#8884);
#399=PLANE('',#8889);
#400=PLANE('',#8900);
#401=PLANE('',#8907);
#402=PLANE('',#8924);
#403=PLANE('',#8929);
#404=PLANE('',#8931);
#405=PLANE('',#8952);
#406=PLANE('',#8955);
#407=PLANE('',#8958);
#408=PLANE('',#8963);
#409=PLANE('',#8967);
#410=PLANE('',#8974);
#411=PLANE('',#8978);
#412=PLANE('',#8979);
#413=PLANE('',#8984);
#414=PLANE('',#8991);
#415=PLANE('',#8993);
#416=PLANE('',#9000);
#417=PLANE('',#9002);
#418=PLANE('',#9005);
#419=PLANE('',#9010);
#420=PLANE('',#9012);
#421=PLANE('',#9015);
#422=PLANE('',#9021);
#423=PLANE('',#9026);
#424=PLANE('',#9028);
#425=PLANE('',#9030);
#426=PLANE('',#9033);
#427=PLANE('',#9035);
#428=PLANE('',#9037);
#429=PLANE('',#9042);
#430=PLANE('',#9050);
#431=PLANE('',#9061);
#432=PLANE('',#9063);
#433=PLANE('',#9066);
#434=PLANE('',#9071);
#435=PLANE('',#9073);
#436=PLANE('',#9076);
#437=PLANE('',#9082);
#438=PLANE('',#9087);
#439=PLANE('',#9089);
#440=PLANE('',#9091);
#441=PLANE('',#9094);
#442=PLANE('',#9096);
#443=PLANE('',#9098);
#444=PLANE('',#9103);
#445=PLANE('',#9111);
#446=PLANE('',#9122);
#447=PLANE('',#9124);
#448=PLANE('',#9127);
#449=PLANE('',#9132);
#450=PLANE('',#9134);
#451=PLANE('',#9137);
#452=PLANE('',#9143);
#453=PLANE('',#9148);
#454=PLANE('',#9150);
#455=PLANE('',#9152);
#456=PLANE('',#9155);
#457=PLANE('',#9157);
#458=PLANE('',#9159);
#459=PLANE('',#9164);
#460=PLANE('',#9172);
#461=PLANE('',#9183);
#462=PLANE('',#9185);
#463=PLANE('',#9188);
#464=PLANE('',#9193);
#465=PLANE('',#9195);
#466=PLANE('',#9198);
#467=PLANE('',#9204);
#468=PLANE('',#9209);
#469=PLANE('',#9211);
#470=PLANE('',#9213);
#471=PLANE('',#9216);
#472=PLANE('',#9218);
#473=PLANE('',#9220);
#474=PLANE('',#9225);
#475=PLANE('',#9233);
#476=FACE_OUTER_BOUND('',#953,.T.);
#477=FACE_OUTER_BOUND('',#954,.T.);
#478=FACE_OUTER_BOUND('',#955,.T.);
#479=FACE_OUTER_BOUND('',#956,.T.);
#480=FACE_OUTER_BOUND('',#957,.T.);
#481=FACE_OUTER_BOUND('',#958,.T.);
#482=FACE_OUTER_BOUND('',#959,.T.);
#483=FACE_OUTER_BOUND('',#960,.T.);
#484=FACE_OUTER_BOUND('',#961,.T.);
#485=FACE_OUTER_BOUND('',#962,.T.);
#486=FACE_OUTER_BOUND('',#963,.T.);
#487=FACE_OUTER_BOUND('',#964,.T.);
#488=FACE_OUTER_BOUND('',#965,.T.);
#489=FACE_OUTER_BOUND('',#966,.T.);
#490=FACE_OUTER_BOUND('',#967,.T.);
#491=FACE_OUTER_BOUND('',#968,.T.);
#492=FACE_OUTER_BOUND('',#969,.T.);
#493=FACE_OUTER_BOUND('',#970,.T.);
#494=FACE_OUTER_BOUND('',#971,.T.);
#495=FACE_OUTER_BOUND('',#972,.T.);
#496=FACE_OUTER_BOUND('',#973,.T.);
#497=FACE_OUTER_BOUND('',#974,.T.);
#498=FACE_OUTER_BOUND('',#975,.T.);
#499=FACE_OUTER_BOUND('',#976,.T.);
#500=FACE_OUTER_BOUND('',#977,.T.);
#501=FACE_OUTER_BOUND('',#978,.T.);
#502=FACE_OUTER_BOUND('',#979,.T.);
#503=FACE_OUTER_BOUND('',#980,.T.);
#504=FACE_OUTER_BOUND('',#981,.T.);
#505=FACE_OUTER_BOUND('',#982,.T.);
#506=FACE_OUTER_BOUND('',#983,.T.);
#507=FACE_OUTER_BOUND('',#984,.T.);
#508=FACE_OUTER_BOUND('',#985,.T.);
#509=FACE_OUTER_BOUND('',#986,.T.);
#510=FACE_OUTER_BOUND('',#987,.T.);
#511=FACE_OUTER_BOUND('',#988,.T.);
#512=FACE_OUTER_BOUND('',#989,.T.);
#513=FACE_OUTER_BOUND('',#990,.T.);
#514=FACE_OUTER_BOUND('',#991,.T.);
#515=FACE_OUTER_BOUND('',#992,.T.);
#516=FACE_OUTER_BOUND('',#993,.T.);
#517=FACE_OUTER_BOUND('',#994,.T.);
#518=FACE_OUTER_BOUND('',#995,.T.);
#519=FACE_OUTER_BOUND('',#996,.T.);
#520=FACE_OUTER_BOUND('',#997,.T.);
#521=FACE_OUTER_BOUND('',#998,.T.);
#522=FACE_OUTER_BOUND('',#999,.T.);
#523=FACE_OUTER_BOUND('',#1000,.T.);
#524=FACE_OUTER_BOUND('',#1001,.T.);
#525=FACE_OUTER_BOUND('',#1002,.T.);
#526=FACE_OUTER_BOUND('',#1003,.T.);
#527=FACE_OUTER_BOUND('',#1004,.T.);
#528=FACE_OUTER_BOUND('',#1005,.T.);
#529=FACE_OUTER_BOUND('',#1006,.T.);
#530=FACE_OUTER_BOUND('',#1007,.T.);
#531=FACE_OUTER_BOUND('',#1008,.T.);
#532=FACE_OUTER_BOUND('',#1009,.T.);
#533=FACE_OUTER_BOUND('',#1010,.T.);
#534=FACE_OUTER_BOUND('',#1011,.T.);
#535=FACE_OUTER_BOUND('',#1012,.T.);
#536=FACE_OUTER_BOUND('',#1013,.T.);
#537=FACE_OUTER_BOUND('',#1014,.T.);
#538=FACE_OUTER_BOUND('',#1015,.T.);
#539=FACE_OUTER_BOUND('',#1016,.T.);
#540=FACE_OUTER_BOUND('',#1017,.T.);
#541=FACE_OUTER_BOUND('',#1018,.T.);
#542=FACE_OUTER_BOUND('',#1019,.T.);
#543=FACE_OUTER_BOUND('',#1020,.T.);
#544=FACE_OUTER_BOUND('',#1021,.T.);
#545=FACE_OUTER_BOUND('',#1022,.T.);
#546=FACE_OUTER_BOUND('',#1023,.T.);
#547=FACE_OUTER_BOUND('',#1024,.T.);
#548=FACE_OUTER_BOUND('',#1025,.T.);
#549=FACE_OUTER_BOUND('',#1026,.T.);
#550=FACE_OUTER_BOUND('',#1027,.T.);
#551=FACE_OUTER_BOUND('',#1028,.T.);
#552=FACE_OUTER_BOUND('',#1029,.T.);
#553=FACE_OUTER_BOUND('',#1030,.T.);
#554=FACE_OUTER_BOUND('',#1031,.T.);
#555=FACE_OUTER_BOUND('',#1032,.T.);
#556=FACE_OUTER_BOUND('',#1033,.T.);
#557=FACE_OUTER_BOUND('',#1034,.T.);
#558=FACE_OUTER_BOUND('',#1035,.T.);
#559=FACE_OUTER_BOUND('',#1036,.T.);
#560=FACE_OUTER_BOUND('',#1037,.T.);
#561=FACE_OUTER_BOUND('',#1038,.T.);
#562=FACE_OUTER_BOUND('',#1039,.T.);
#563=FACE_OUTER_BOUND('',#1040,.T.);
#564=FACE_OUTER_BOUND('',#1041,.T.);
#565=FACE_OUTER_BOUND('',#1042,.T.);
#566=FACE_OUTER_BOUND('',#1044,.T.);
#567=FACE_OUTER_BOUND('',#1046,.T.);
#568=FACE_OUTER_BOUND('',#1047,.T.);
#569=FACE_OUTER_BOUND('',#1048,.T.);
#570=FACE_OUTER_BOUND('',#1049,.T.);
#571=FACE_OUTER_BOUND('',#1051,.T.);
#572=FACE_OUTER_BOUND('',#1053,.T.);
#573=FACE_OUTER_BOUND('',#1054,.T.);
#574=FACE_OUTER_BOUND('',#1055,.T.);
#575=FACE_OUTER_BOUND('',#1056,.T.);
#576=FACE_OUTER_BOUND('',#1057,.T.);
#577=FACE_OUTER_BOUND('',#1058,.T.);
#578=FACE_OUTER_BOUND('',#1061,.T.);
#579=FACE_OUTER_BOUND('',#1062,.T.);
#580=FACE_OUTER_BOUND('',#1063,.T.);
#581=FACE_OUTER_BOUND('',#1064,.T.);
#582=FACE_OUTER_BOUND('',#1065,.T.);
#583=FACE_OUTER_BOUND('',#1066,.T.);
#584=FACE_OUTER_BOUND('',#1067,.T.);
#585=FACE_OUTER_BOUND('',#1068,.T.);
#586=FACE_OUTER_BOUND('',#1069,.T.);
#587=FACE_OUTER_BOUND('',#1070,.T.);
#588=FACE_OUTER_BOUND('',#1072,.T.);
#589=FACE_OUTER_BOUND('',#1073,.T.);
#590=FACE_OUTER_BOUND('',#1074,.T.);
#591=FACE_OUTER_BOUND('',#1075,.T.);
#592=FACE_OUTER_BOUND('',#1076,.T.);
#593=FACE_OUTER_BOUND('',#1077,.T.);
#594=FACE_OUTER_BOUND('',#1078,.T.);
#595=FACE_OUTER_BOUND('',#1080,.T.);
#596=FACE_OUTER_BOUND('',#1081,.T.);
#597=FACE_OUTER_BOUND('',#1082,.T.);
#598=FACE_OUTER_BOUND('',#1083,.T.);
#599=FACE_OUTER_BOUND('',#1084,.T.);
#600=FACE_OUTER_BOUND('',#1087,.T.);
#601=FACE_OUTER_BOUND('',#1088,.T.);
#602=FACE_OUTER_BOUND('',#1089,.T.);
#603=FACE_OUTER_BOUND('',#1090,.T.);
#604=FACE_OUTER_BOUND('',#1091,.T.);
#605=FACE_OUTER_BOUND('',#1092,.T.);
#606=FACE_OUTER_BOUND('',#1093,.T.);
#607=FACE_OUTER_BOUND('',#1094,.T.);
#608=FACE_OUTER_BOUND('',#1095,.T.);
#609=FACE_OUTER_BOUND('',#1096,.T.);
#610=FACE_OUTER_BOUND('',#1097,.T.);
#611=FACE_OUTER_BOUND('',#1098,.T.);
#612=FACE_OUTER_BOUND('',#1099,.T.);
#613=FACE_OUTER_BOUND('',#1100,.T.);
#614=FACE_OUTER_BOUND('',#1101,.T.);
#615=FACE_OUTER_BOUND('',#1102,.T.);
#616=FACE_OUTER_BOUND('',#1103,.T.);
#617=FACE_OUTER_BOUND('',#1104,.T.);
#618=FACE_OUTER_BOUND('',#1105,.T.);
#619=FACE_OUTER_BOUND('',#1106,.T.);
#620=FACE_OUTER_BOUND('',#1107,.T.);
#621=FACE_OUTER_BOUND('',#1108,.T.);
#622=FACE_OUTER_BOUND('',#1109,.T.);
#623=FACE_OUTER_BOUND('',#1110,.T.);
#624=FACE_OUTER_BOUND('',#1111,.T.);
#625=FACE_OUTER_BOUND('',#1112,.T.);
#626=FACE_OUTER_BOUND('',#1113,.T.);
#627=FACE_OUTER_BOUND('',#1114,.T.);
#628=FACE_OUTER_BOUND('',#1115,.T.);
#629=FACE_OUTER_BOUND('',#1116,.T.);
#630=FACE_OUTER_BOUND('',#1117,.T.);
#631=FACE_OUTER_BOUND('',#1118,.T.);
#632=FACE_OUTER_BOUND('',#1119,.T.);
#633=FACE_OUTER_BOUND('',#1120,.T.);
#634=FACE_OUTER_BOUND('',#1121,.T.);
#635=FACE_OUTER_BOUND('',#1122,.T.);
#636=FACE_OUTER_BOUND('',#1123,.T.);
#637=FACE_OUTER_BOUND('',#1124,.T.);
#638=FACE_OUTER_BOUND('',#1125,.T.);
#639=FACE_OUTER_BOUND('',#1126,.T.);
#640=FACE_OUTER_BOUND('',#1127,.T.);
#641=FACE_OUTER_BOUND('',#1128,.T.);
#642=FACE_OUTER_BOUND('',#1129,.T.);
#643=FACE_OUTER_BOUND('',#1130,.T.);
#644=FACE_OUTER_BOUND('',#1131,.T.);
#645=FACE_OUTER_BOUND('',#1132,.T.);
#646=FACE_OUTER_BOUND('',#1133,.T.);
#647=FACE_OUTER_BOUND('',#1134,.T.);
#648=FACE_OUTER_BOUND('',#1135,.T.);
#649=FACE_OUTER_BOUND('',#1136,.T.);
#650=FACE_OUTER_BOUND('',#1137,.T.);
#651=FACE_OUTER_BOUND('',#1138,.T.);
#652=FACE_OUTER_BOUND('',#1139,.T.);
#653=FACE_OUTER_BOUND('',#1140,.T.);
#654=FACE_OUTER_BOUND('',#1142,.T.);
#655=FACE_OUTER_BOUND('',#1143,.T.);
#656=FACE_OUTER_BOUND('',#1144,.T.);
#657=FACE_OUTER_BOUND('',#1147,.T.);
#658=FACE_OUTER_BOUND('',#1148,.T.);
#659=FACE_OUTER_BOUND('',#1149,.T.);
#660=FACE_OUTER_BOUND('',#1150,.T.);
#661=FACE_OUTER_BOUND('',#1153,.T.);
#662=FACE_OUTER_BOUND('',#1154,.T.);
#663=FACE_OUTER_BOUND('',#1155,.T.);
#664=FACE_OUTER_BOUND('',#1156,.T.);
#665=FACE_OUTER_BOUND('',#1159,.T.);
#666=FACE_OUTER_BOUND('',#1160,.T.);
#667=FACE_OUTER_BOUND('',#1161,.T.);
#668=FACE_OUTER_BOUND('',#1162,.T.);
#669=FACE_OUTER_BOUND('',#1165,.T.);
#670=FACE_OUTER_BOUND('',#1166,.T.);
#671=FACE_OUTER_BOUND('',#1168,.T.);
#672=FACE_OUTER_BOUND('',#1169,.T.);
#673=FACE_OUTER_BOUND('',#1170,.T.);
#674=FACE_OUTER_BOUND('',#1171,.T.);
#675=FACE_OUTER_BOUND('',#1172,.T.);
#676=FACE_OUTER_BOUND('',#1173,.T.);
#677=FACE_OUTER_BOUND('',#1174,.T.);
#678=FACE_OUTER_BOUND('',#1175,.T.);
#679=FACE_OUTER_BOUND('',#1176,.T.);
#680=FACE_OUTER_BOUND('',#1177,.T.);
#681=FACE_OUTER_BOUND('',#1178,.T.);
#682=FACE_OUTER_BOUND('',#1179,.T.);
#683=FACE_OUTER_BOUND('',#1180,.T.);
#684=FACE_OUTER_BOUND('',#1182,.T.);
#685=FACE_OUTER_BOUND('',#1183,.T.);
#686=FACE_OUTER_BOUND('',#1184,.T.);
#687=FACE_OUTER_BOUND('',#1185,.T.);
#688=FACE_OUTER_BOUND('',#1186,.T.);
#689=FACE_OUTER_BOUND('',#1187,.T.);
#690=FACE_OUTER_BOUND('',#1188,.T.);
#691=FACE_OUTER_BOUND('',#1189,.T.);
#692=FACE_OUTER_BOUND('',#1190,.T.);
#693=FACE_OUTER_BOUND('',#1191,.T.);
#694=FACE_OUTER_BOUND('',#1192,.T.);
#695=FACE_OUTER_BOUND('',#1193,.T.);
#696=FACE_OUTER_BOUND('',#1194,.T.);
#697=FACE_OUTER_BOUND('',#1195,.T.);
#698=FACE_OUTER_BOUND('',#1196,.T.);
#699=FACE_OUTER_BOUND('',#1197,.T.);
#700=FACE_OUTER_BOUND('',#1198,.T.);
#701=FACE_OUTER_BOUND('',#1199,.T.);
#702=FACE_OUTER_BOUND('',#1200,.T.);
#703=FACE_OUTER_BOUND('',#1201,.T.);
#704=FACE_OUTER_BOUND('',#1202,.T.);
#705=FACE_OUTER_BOUND('',#1203,.T.);
#706=FACE_OUTER_BOUND('',#1204,.T.);
#707=FACE_OUTER_BOUND('',#1205,.T.);
#708=FACE_OUTER_BOUND('',#1206,.T.);
#709=FACE_OUTER_BOUND('',#1207,.T.);
#710=FACE_OUTER_BOUND('',#1208,.T.);
#711=FACE_OUTER_BOUND('',#1209,.T.);
#712=FACE_OUTER_BOUND('',#1210,.T.);
#713=FACE_OUTER_BOUND('',#1211,.T.);
#714=FACE_OUTER_BOUND('',#1212,.T.);
#715=FACE_OUTER_BOUND('',#1213,.T.);
#716=FACE_OUTER_BOUND('',#1214,.T.);
#717=FACE_OUTER_BOUND('',#1215,.T.);
#718=FACE_OUTER_BOUND('',#1216,.T.);
#719=FACE_OUTER_BOUND('',#1217,.T.);
#720=FACE_OUTER_BOUND('',#1218,.T.);
#721=FACE_OUTER_BOUND('',#1219,.T.);
#722=FACE_OUTER_BOUND('',#1220,.T.);
#723=FACE_OUTER_BOUND('',#1221,.T.);
#724=FACE_OUTER_BOUND('',#1222,.T.);
#725=FACE_OUTER_BOUND('',#1223,.T.);
#726=FACE_OUTER_BOUND('',#1224,.T.);
#727=FACE_OUTER_BOUND('',#1225,.T.);
#728=FACE_OUTER_BOUND('',#1226,.T.);
#729=FACE_OUTER_BOUND('',#1227,.T.);
#730=FACE_OUTER_BOUND('',#1229,.T.);
#731=FACE_OUTER_BOUND('',#1230,.T.);
#732=FACE_OUTER_BOUND('',#1231,.T.);
#733=FACE_OUTER_BOUND('',#1232,.T.);
#734=FACE_OUTER_BOUND('',#1233,.T.);
#735=FACE_OUTER_BOUND('',#1234,.T.);
#736=FACE_OUTER_BOUND('',#1235,.T.);
#737=FACE_OUTER_BOUND('',#1236,.T.);
#738=FACE_OUTER_BOUND('',#1238,.T.);
#739=FACE_OUTER_BOUND('',#1239,.T.);
#740=FACE_OUTER_BOUND('',#1240,.T.);
#741=FACE_OUTER_BOUND('',#1241,.T.);
#742=FACE_OUTER_BOUND('',#1242,.T.);
#743=FACE_OUTER_BOUND('',#1243,.T.);
#744=FACE_OUTER_BOUND('',#1244,.T.);
#745=FACE_OUTER_BOUND('',#1245,.T.);
#746=FACE_OUTER_BOUND('',#1246,.T.);
#747=FACE_OUTER_BOUND('',#1247,.T.);
#748=FACE_OUTER_BOUND('',#1248,.T.);
#749=FACE_OUTER_BOUND('',#1249,.T.);
#750=FACE_OUTER_BOUND('',#1250,.T.);
#751=FACE_OUTER_BOUND('',#1251,.T.);
#752=FACE_OUTER_BOUND('',#1252,.T.);
#753=FACE_OUTER_BOUND('',#1253,.T.);
#754=FACE_OUTER_BOUND('',#1254,.T.);
#755=FACE_OUTER_BOUND('',#1255,.T.);
#756=FACE_OUTER_BOUND('',#1256,.T.);
#757=FACE_OUTER_BOUND('',#1257,.T.);
#758=FACE_OUTER_BOUND('',#1258,.T.);
#759=FACE_OUTER_BOUND('',#1259,.T.);
#760=FACE_OUTER_BOUND('',#1261,.T.);
#761=FACE_OUTER_BOUND('',#1262,.T.);
#762=FACE_OUTER_BOUND('',#1263,.T.);
#763=FACE_OUTER_BOUND('',#1265,.T.);
#764=FACE_OUTER_BOUND('',#1266,.T.);
#765=FACE_OUTER_BOUND('',#1268,.T.);
#766=FACE_OUTER_BOUND('',#1269,.T.);
#767=FACE_OUTER_BOUND('',#1270,.T.);
#768=FACE_OUTER_BOUND('',#1271,.T.);
#769=FACE_OUTER_BOUND('',#1272,.T.);
#770=FACE_OUTER_BOUND('',#1273,.T.);
#771=FACE_OUTER_BOUND('',#1274,.T.);
#772=FACE_OUTER_BOUND('',#1275,.T.);
#773=FACE_OUTER_BOUND('',#1276,.T.);
#774=FACE_OUTER_BOUND('',#1277,.T.);
#775=FACE_OUTER_BOUND('',#1278,.T.);
#776=FACE_OUTER_BOUND('',#1279,.T.);
#777=FACE_OUTER_BOUND('',#1280,.T.);
#778=FACE_OUTER_BOUND('',#1282,.T.);
#779=FACE_OUTER_BOUND('',#1283,.T.);
#780=FACE_OUTER_BOUND('',#1284,.T.);
#781=FACE_OUTER_BOUND('',#1285,.T.);
#782=FACE_OUTER_BOUND('',#1286,.T.);
#783=FACE_OUTER_BOUND('',#1287,.T.);
#784=FACE_OUTER_BOUND('',#1288,.T.);
#785=FACE_OUTER_BOUND('',#1289,.T.);
#786=FACE_OUTER_BOUND('',#1290,.T.);
#787=FACE_OUTER_BOUND('',#1291,.T.);
#788=FACE_OUTER_BOUND('',#1292,.T.);
#789=FACE_OUTER_BOUND('',#1293,.T.);
#790=FACE_OUTER_BOUND('',#1295,.T.);
#791=FACE_OUTER_BOUND('',#1296,.T.);
#792=FACE_OUTER_BOUND('',#1297,.T.);
#793=FACE_OUTER_BOUND('',#1298,.T.);
#794=FACE_OUTER_BOUND('',#1300,.T.);
#795=FACE_OUTER_BOUND('',#1301,.T.);
#796=FACE_OUTER_BOUND('',#1302,.T.);
#797=FACE_OUTER_BOUND('',#1303,.T.);
#798=FACE_OUTER_BOUND('',#1305,.T.);
#799=FACE_OUTER_BOUND('',#1306,.T.);
#800=FACE_OUTER_BOUND('',#1307,.T.);
#801=FACE_OUTER_BOUND('',#1308,.T.);
#802=FACE_OUTER_BOUND('',#1309,.T.);
#803=FACE_OUTER_BOUND('',#1310,.T.);
#804=FACE_OUTER_BOUND('',#1311,.T.);
#805=FACE_OUTER_BOUND('',#1312,.T.);
#806=FACE_OUTER_BOUND('',#1313,.T.);
#807=FACE_OUTER_BOUND('',#1314,.T.);
#808=FACE_OUTER_BOUND('',#1315,.T.);
#809=FACE_OUTER_BOUND('',#1316,.T.);
#810=FACE_OUTER_BOUND('',#1317,.T.);
#811=FACE_OUTER_BOUND('',#1318,.T.);
#812=FACE_OUTER_BOUND('',#1319,.T.);
#813=FACE_OUTER_BOUND('',#1320,.T.);
#814=FACE_OUTER_BOUND('',#1321,.T.);
#815=FACE_OUTER_BOUND('',#1322,.T.);
#816=FACE_OUTER_BOUND('',#1323,.T.);
#817=FACE_OUTER_BOUND('',#1325,.T.);
#818=FACE_OUTER_BOUND('',#1326,.T.);
#819=FACE_OUTER_BOUND('',#1328,.T.);
#820=FACE_OUTER_BOUND('',#1330,.T.);
#821=FACE_OUTER_BOUND('',#1331,.T.);
#822=FACE_OUTER_BOUND('',#1332,.T.);
#823=FACE_OUTER_BOUND('',#1333,.T.);
#824=FACE_OUTER_BOUND('',#1334,.T.);
#825=FACE_OUTER_BOUND('',#1335,.T.);
#826=FACE_OUTER_BOUND('',#1336,.T.);
#827=FACE_OUTER_BOUND('',#1337,.T.);
#828=FACE_OUTER_BOUND('',#1338,.T.);
#829=FACE_OUTER_BOUND('',#1339,.T.);
#830=FACE_OUTER_BOUND('',#1340,.T.);
#831=FACE_OUTER_BOUND('',#1341,.T.);
#832=FACE_OUTER_BOUND('',#1342,.T.);
#833=FACE_OUTER_BOUND('',#1343,.T.);
#834=FACE_OUTER_BOUND('',#1344,.T.);
#835=FACE_OUTER_BOUND('',#1346,.T.);
#836=FACE_OUTER_BOUND('',#1347,.T.);
#837=FACE_OUTER_BOUND('',#1348,.T.);
#838=FACE_OUTER_BOUND('',#1349,.T.);
#839=FACE_OUTER_BOUND('',#1350,.T.);
#840=FACE_OUTER_BOUND('',#1351,.T.);
#841=FACE_OUTER_BOUND('',#1352,.T.);
#842=FACE_OUTER_BOUND('',#1353,.T.);
#843=FACE_OUTER_BOUND('',#1354,.T.);
#844=FACE_OUTER_BOUND('',#1356,.T.);
#845=FACE_OUTER_BOUND('',#1358,.T.);
#846=FACE_OUTER_BOUND('',#1359,.T.);
#847=FACE_OUTER_BOUND('',#1360,.T.);
#848=FACE_OUTER_BOUND('',#1361,.T.);
#849=FACE_OUTER_BOUND('',#1362,.T.);
#850=FACE_OUTER_BOUND('',#1363,.T.);
#851=FACE_OUTER_BOUND('',#1364,.T.);
#852=FACE_OUTER_BOUND('',#1365,.T.);
#853=FACE_OUTER_BOUND('',#1366,.T.);
#854=FACE_OUTER_BOUND('',#1367,.T.);
#855=FACE_OUTER_BOUND('',#1368,.T.);
#856=FACE_OUTER_BOUND('',#1369,.T.);
#857=FACE_OUTER_BOUND('',#1370,.T.);
#858=FACE_OUTER_BOUND('',#1371,.T.);
#859=FACE_OUTER_BOUND('',#1372,.T.);
#860=FACE_OUTER_BOUND('',#1373,.T.);
#861=FACE_OUTER_BOUND('',#1374,.T.);
#862=FACE_OUTER_BOUND('',#1375,.T.);
#863=FACE_OUTER_BOUND('',#1376,.T.);
#864=FACE_OUTER_BOUND('',#1377,.T.);
#865=FACE_OUTER_BOUND('',#1378,.T.);
#866=FACE_OUTER_BOUND('',#1379,.T.);
#867=FACE_OUTER_BOUND('',#1380,.T.);
#868=FACE_OUTER_BOUND('',#1381,.T.);
#869=FACE_OUTER_BOUND('',#1382,.T.);
#870=FACE_OUTER_BOUND('',#1383,.T.);
#871=FACE_OUTER_BOUND('',#1384,.T.);
#872=FACE_OUTER_BOUND('',#1386,.T.);
#873=FACE_OUTER_BOUND('',#1387,.T.);
#874=FACE_OUTER_BOUND('',#1388,.T.);
#875=FACE_OUTER_BOUND('',#1389,.T.);
#876=FACE_OUTER_BOUND('',#1390,.T.);
#877=FACE_OUTER_BOUND('',#1391,.T.);
#878=FACE_OUTER_BOUND('',#1392,.T.);
#879=FACE_OUTER_BOUND('',#1393,.T.);
#880=FACE_OUTER_BOUND('',#1394,.T.);
#881=FACE_OUTER_BOUND('',#1395,.T.);
#882=FACE_OUTER_BOUND('',#1396,.T.);
#883=FACE_OUTER_BOUND('',#1397,.T.);
#884=FACE_OUTER_BOUND('',#1398,.T.);
#885=FACE_OUTER_BOUND('',#1399,.T.);
#886=FACE_OUTER_BOUND('',#1400,.T.);
#887=FACE_OUTER_BOUND('',#1401,.T.);
#888=FACE_OUTER_BOUND('',#1402,.T.);
#889=FACE_OUTER_BOUND('',#1403,.T.);
#890=FACE_OUTER_BOUND('',#1404,.T.);
#891=FACE_OUTER_BOUND('',#1405,.T.);
#892=FACE_OUTER_BOUND('',#1406,.T.);
#893=FACE_OUTER_BOUND('',#1407,.T.);
#894=FACE_OUTER_BOUND('',#1408,.T.);
#895=FACE_OUTER_BOUND('',#1409,.T.);
#896=FACE_OUTER_BOUND('',#1410,.T.);
#897=FACE_OUTER_BOUND('',#1412,.T.);
#898=FACE_OUTER_BOUND('',#1413,.T.);
#899=FACE_OUTER_BOUND('',#1414,.T.);
#900=FACE_OUTER_BOUND('',#1415,.T.);
#901=FACE_OUTER_BOUND('',#1416,.T.);
#902=FACE_OUTER_BOUND('',#1417,.T.);
#903=FACE_OUTER_BOUND('',#1418,.T.);
#904=FACE_OUTER_BOUND('',#1419,.T.);
#905=FACE_OUTER_BOUND('',#1420,.T.);
#906=FACE_OUTER_BOUND('',#1421,.T.);
#907=FACE_OUTER_BOUND('',#1422,.T.);
#908=FACE_OUTER_BOUND('',#1423,.T.);
#909=FACE_OUTER_BOUND('',#1424,.T.);
#910=FACE_OUTER_BOUND('',#1425,.T.);
#911=FACE_OUTER_BOUND('',#1426,.T.);
#912=FACE_OUTER_BOUND('',#1427,.T.);
#913=FACE_OUTER_BOUND('',#1428,.T.);
#914=FACE_OUTER_BOUND('',#1429,.T.);
#915=FACE_OUTER_BOUND('',#1430,.T.);
#916=FACE_OUTER_BOUND('',#1431,.T.);
#917=FACE_OUTER_BOUND('',#1432,.T.);
#918=FACE_OUTER_BOUND('',#1433,.T.);
#919=FACE_OUTER_BOUND('',#1434,.T.);
#920=FACE_OUTER_BOUND('',#1435,.T.);
#921=FACE_OUTER_BOUND('',#1436,.T.);
#922=FACE_OUTER_BOUND('',#1438,.T.);
#923=FACE_OUTER_BOUND('',#1439,.T.);
#924=FACE_OUTER_BOUND('',#1440,.T.);
#925=FACE_OUTER_BOUND('',#1441,.T.);
#926=FACE_OUTER_BOUND('',#1442,.T.);
#927=FACE_OUTER_BOUND('',#1443,.T.);
#928=FACE_OUTER_BOUND('',#1444,.T.);
#929=FACE_OUTER_BOUND('',#1445,.T.);
#930=FACE_OUTER_BOUND('',#1446,.T.);
#931=FACE_OUTER_BOUND('',#1447,.T.);
#932=FACE_OUTER_BOUND('',#1448,.T.);
#933=FACE_OUTER_BOUND('',#1449,.T.);
#934=FACE_OUTER_BOUND('',#1450,.T.);
#935=FACE_OUTER_BOUND('',#1451,.T.);
#936=FACE_OUTER_BOUND('',#1452,.T.);
#937=FACE_OUTER_BOUND('',#1453,.T.);
#938=FACE_OUTER_BOUND('',#1454,.T.);
#939=FACE_OUTER_BOUND('',#1455,.T.);
#940=FACE_OUTER_BOUND('',#1456,.T.);
#941=FACE_OUTER_BOUND('',#1457,.T.);
#942=FACE_OUTER_BOUND('',#1458,.T.);
#943=FACE_OUTER_BOUND('',#1459,.T.);
#944=FACE_OUTER_BOUND('',#1460,.T.);
#945=FACE_OUTER_BOUND('',#1461,.T.);
#946=FACE_OUTER_BOUND('',#1462,.T.);
#947=FACE_OUTER_BOUND('',#1464,.T.);
#948=FACE_OUTER_BOUND('',#1465,.T.);
#949=FACE_OUTER_BOUND('',#1466,.T.);
#950=FACE_OUTER_BOUND('',#1467,.T.);
#951=FACE_OUTER_BOUND('',#1468,.T.);
#952=FACE_OUTER_BOUND('',#1469,.T.);
#953=EDGE_LOOP('',(#5089,#5090,#5091,#5092,#5093,#5094,#5095));
#954=EDGE_LOOP('',(#5096,#5097,#5098,#5099));
#955=EDGE_LOOP('',(#5100,#5101,#5102,#5103,#5104,#5105));
#956=EDGE_LOOP('',(#5106,#5107,#5108,#5109));
#957=EDGE_LOOP('',(#5110,#5111,#5112,#5113,#5114,#5115));
#958=EDGE_LOOP('',(#5116,#5117,#5118,#5119));
#959=EDGE_LOOP('',(#5120,#5121,#5122,#5123));
#960=EDGE_LOOP('',(#5124,#5125,#5126,#5127));
#961=EDGE_LOOP('',(#5128,#5129,#5130,#5131,#5132,#5133,#5134,#5135,#5136));
#962=EDGE_LOOP('',(#5137,#5138,#5139,#5140,#5141,#5142,#5143,#5144,#5145,
#5146,#5147,#5148,#5149,#5150,#5151));
#963=EDGE_LOOP('',(#5152,#5153,#5154,#5155));
#964=EDGE_LOOP('',(#5156,#5157,#5158,#5159));
#965=EDGE_LOOP('',(#5160,#5161,#5162,#5163));
#966=EDGE_LOOP('',(#5164,#5165,#5166,#5167));
#967=EDGE_LOOP('',(#5168,#5169,#5170,#5171));
#968=EDGE_LOOP('',(#5172,#5173,#5174,#5175));
#969=EDGE_LOOP('',(#5176,#5177,#5178,#5179));
#970=EDGE_LOOP('',(#5180,#5181,#5182,#5183));
#971=EDGE_LOOP('',(#5184,#5185,#5186));
#972=EDGE_LOOP('',(#5187,#5188,#5189,#5190));
#973=EDGE_LOOP('',(#5191,#5192,#5193));
#974=EDGE_LOOP('',(#5194,#5195,#5196,#5197,#5198,#5199,#5200,#5201,#5202,
#5203));
#975=EDGE_LOOP('',(#5204,#5205,#5206,#5207));
#976=EDGE_LOOP('',(#5208,#5209,#5210,#5211,#5212,#5213,#5214,#5215,#5216,
#5217,#5218,#5219,#5220,#5221,#5222,#5223,#5224,#5225,#5226,#5227));
#977=EDGE_LOOP('',(#5228,#5229,#5230,#5231));
#978=EDGE_LOOP('',(#5232,#5233,#5234,#5235,#5236,#5237,#5238,#5239));
#979=EDGE_LOOP('',(#5240,#5241,#5242,#5243));
#980=EDGE_LOOP('',(#5244,#5245,#5246,#5247));
#981=EDGE_LOOP('',(#5248,#5249,#5250,#5251));
#982=EDGE_LOOP('',(#5252,#5253,#5254,#5255));
#983=EDGE_LOOP('',(#5256,#5257,#5258,#5259));
#984=EDGE_LOOP('',(#5260,#5261,#5262,#5263,#5264,#5265,#5266,#5267,#5268,
#5269));
#985=EDGE_LOOP('',(#5270,#5271,#5272,#5273,#5274,#5275,#5276,#5277,#5278,
#5279,#5280,#5281,#5282,#5283,#5284,#5285,#5286,#5287,#5288));
#986=EDGE_LOOP('',(#5289,#5290,#5291,#5292,#5293,#5294,#5295,#5296));
#987=EDGE_LOOP('',(#5297,#5298,#5299,#5300,#5301,#5302,#5303,#5304));
#988=EDGE_LOOP('',(#5305,#5306,#5307,#5308,#5309,#5310,#5311,#5312));
#989=EDGE_LOOP('',(#5313,#5314,#5315,#5316,#5317,#5318,#5319,#5320));
#990=EDGE_LOOP('',(#5321,#5322,#5323,#5324));
#991=EDGE_LOOP('',(#5325,#5326,#5327,#5328,#5329,#5330,#5331));
#992=EDGE_LOOP('',(#5332,#5333,#5334,#5335,#5336,#5337));
#993=EDGE_LOOP('',(#5338,#5339,#5340,#5341,#5342,#5343));
#994=EDGE_LOOP('',(#5344,#5345,#5346,#5347,#5348,#5349,#5350,#5351));
#995=EDGE_LOOP('',(#5352,#5353,#5354,#5355));
#996=EDGE_LOOP('',(#5356,#5357,#5358,#5359,#5360,#5361,#5362,#5363,#5364,
#5365));
#997=EDGE_LOOP('',(#5366,#5367,#5368,#5369,#5370,#5371,#5372,#5373,#5374,
#5375,#5376,#5377,#5378,#5379,#5380,#5381,#5382,#5383));
#998=EDGE_LOOP('',(#5384,#5385,#5386,#5387));
#999=EDGE_LOOP('',(#5388,#5389,#5390,#5391,#5392,#5393));
#1000=EDGE_LOOP('',(#5394,#5395,#5396,#5397));
#1001=EDGE_LOOP('',(#5398,#5399,#5400,#5401));
#1002=EDGE_LOOP('',(#5402,#5403,#5404,#5405));
#1003=EDGE_LOOP('',(#5406,#5407,#5408,#5409,#5410,#5411,#5412));
#1004=EDGE_LOOP('',(#5413,#5414,#5415,#5416,#5417,#5418,#5419,#5420));
#1005=EDGE_LOOP('',(#5421,#5422,#5423,#5424));
#1006=EDGE_LOOP('',(#5425,#5426,#5427,#5428));
#1007=EDGE_LOOP('',(#5429,#5430,#5431,#5432));
#1008=EDGE_LOOP('',(#5433,#5434,#5435,#5436));
#1009=EDGE_LOOP('',(#5437,#5438,#5439,#5440,#5441,#5442));
#1010=EDGE_LOOP('',(#5443,#5444,#5445,#5446));
#1011=EDGE_LOOP('',(#5447,#5448,#5449,#5450));
#1012=EDGE_LOOP('',(#5451,#5452,#5453,#5454));
#1013=EDGE_LOOP('',(#5455,#5456,#5457,#5458));
#1014=EDGE_LOOP('',(#5459,#5460,#5461,#5462));
#1015=EDGE_LOOP('',(#5463,#5464,#5465,#5466));
#1016=EDGE_LOOP('',(#5467,#5468,#5469,#5470));
#1017=EDGE_LOOP('',(#5471,#5472,#5473,#5474));
#1018=EDGE_LOOP('',(#5475,#5476,#5477,#5478));
#1019=EDGE_LOOP('',(#5479,#5480,#5481,#5482));
#1020=EDGE_LOOP('',(#5483,#5484,#5485,#5486));
#1021=EDGE_LOOP('',(#5487,#5488,#5489,#5490));
#1022=EDGE_LOOP('',(#5491,#5492,#5493));
#1023=EDGE_LOOP('',(#5494,#5495,#5496));
#1024=EDGE_LOOP('',(#5497,#5498,#5499));
#1025=EDGE_LOOP('',(#5500,#5501,#5502));
#1026=EDGE_LOOP('',(#5503,#5504,#5505,#5506));
#1027=EDGE_LOOP('',(#5507,#5508,#5509,#5510));
#1028=EDGE_LOOP('',(#5511,#5512,#5513,#5514));
#1029=EDGE_LOOP('',(#5515,#5516,#5517,#5518));
#1030=EDGE_LOOP('',(#5519,#5520,#5521,#5522));
#1031=EDGE_LOOP('',(#5523,#5524,#5525,#5526));
#1032=EDGE_LOOP('',(#5527,#5528,#5529,#5530));
#1033=EDGE_LOOP('',(#5531,#5532,#5533,#5534));
#1034=EDGE_LOOP('',(#5535,#5536,#5537,#5538,#5539,#5540));
#1035=EDGE_LOOP('',(#5541,#5542,#5543,#5544));
#1036=EDGE_LOOP('',(#5545,#5546,#5547,#5548));
#1037=EDGE_LOOP('',(#5549,#5550,#5551,#5552));
#1038=EDGE_LOOP('',(#5553,#5554,#5555,#5556));
#1039=EDGE_LOOP('',(#5557,#5558,#5559,#5560));
#1040=EDGE_LOOP('',(#5561,#5562,#5563,#5564));
#1041=EDGE_LOOP('',(#5565,#5566,#5567,#5568));
#1042=EDGE_LOOP('',(#5569,#5570,#5571,#5572,#5573,#5574,#5575));
#1043=EDGE_LOOP('',(#5576));
#1044=EDGE_LOOP('',(#5577,#5578,#5579,#5580,#5581,#5582,#5583,#5584));
#1045=EDGE_LOOP('',(#5585));
#1046=EDGE_LOOP('',(#5586,#5587,#5588,#5589));
#1047=EDGE_LOOP('',(#5590,#5591,#5592,#5593));
#1048=EDGE_LOOP('',(#5594,#5595,#5596,#5597));
#1049=EDGE_LOOP('',(#5598,#5599,#5600,#5601,#5602,#5603,#5604));
#1050=EDGE_LOOP('',(#5605));
#1051=EDGE_LOOP('',(#5606,#5607,#5608,#5609,#5610,#5611));
#1052=EDGE_LOOP('',(#5612));
#1053=EDGE_LOOP('',(#5613,#5614,#5615,#5616));
#1054=EDGE_LOOP('',(#5617,#5618,#5619,#5620,#5621,#5622,#5623,#5624,#5625,
#5626,#5627,#5628,#5629,#5630));
#1055=EDGE_LOOP('',(#5631,#5632,#5633,#5634));
#1056=EDGE_LOOP('',(#5635,#5636,#5637,#5638));
#1057=EDGE_LOOP('',(#5639,#5640,#5641,#5642));
#1058=EDGE_LOOP('',(#5643,#5644,#5645,#5646,#5647,#5648,#5649,#5650,#5651,
#5652,#5653,#5654,#5655,#5656,#5657,#5658,#5659));
#1059=EDGE_LOOP('',(#5660));
#1060=EDGE_LOOP('',(#5661));
#1061=EDGE_LOOP('',(#5662,#5663,#5664,#5665));
#1062=EDGE_LOOP('',(#5666,#5667,#5668,#5669));
#1063=EDGE_LOOP('',(#5670,#5671,#5672,#5673));
#1064=EDGE_LOOP('',(#5674,#5675,#5676,#5677));
#1065=EDGE_LOOP('',(#5678,#5679,#5680,#5681));
#1066=EDGE_LOOP('',(#5682,#5683,#5684,#5685));
#1067=EDGE_LOOP('',(#5686,#5687,#5688,#5689));
#1068=EDGE_LOOP('',(#5690,#5691,#5692,#5693));
#1069=EDGE_LOOP('',(#5694,#5695,#5696,#5697,#5698));
#1070=EDGE_LOOP('',(#5699,#5700,#5701,#5702));
#1071=EDGE_LOOP('',(#5703));
#1072=EDGE_LOOP('',(#5704,#5705,#5706,#5707,#5708,#5709,#5710));
#1073=EDGE_LOOP('',(#5711,#5712,#5713,#5714));
#1074=EDGE_LOOP('',(#5715,#5716,#5717,#5718));
#1075=EDGE_LOOP('',(#5719,#5720,#5721,#5722,#5723,#5724,#5725));
#1076=EDGE_LOOP('',(#5726,#5727,#5728,#5729,#5730,#5731,#5732,#5733,#5734,
#5735,#5736,#5737,#5738,#5739,#5740));
#1077=EDGE_LOOP('',(#5741,#5742,#5743,#5744));
#1078=EDGE_LOOP('',(#5745,#5746,#5747,#5748));
#1079=EDGE_LOOP('',(#5749));
#1080=EDGE_LOOP('',(#5750,#5751,#5752,#5753));
#1081=EDGE_LOOP('',(#5754,#5755,#5756,#5757));
#1082=EDGE_LOOP('',(#5758,#5759,#5760,#5761,#5762));
#1083=EDGE_LOOP('',(#5763,#5764,#5765,#5766));
#1084=EDGE_LOOP('',(#5767,#5768,#5769,#5770,#5771,#5772,#5773,#5774,#5775,
#5776,#5777,#5778,#5779,#5780,#5781));
#1085=EDGE_LOOP('',(#5782));
#1086=EDGE_LOOP('',(#5783));
#1087=EDGE_LOOP('',(#5784,#5785,#5786,#5787));
#1088=EDGE_LOOP('',(#5788,#5789,#5790,#5791));
#1089=EDGE_LOOP('',(#5792,#5793,#5794,#5795));
#1090=EDGE_LOOP('',(#5796,#5797,#5798,#5799));
#1091=EDGE_LOOP('',(#5800,#5801,#5802,#5803));
#1092=EDGE_LOOP('',(#5804,#5805,#5806,#5807,#5808,#5809,#5810,#5811,#5812,
#5813));
#1093=EDGE_LOOP('',(#5814,#5815,#5816,#5817,#5818,#5819,#5820,#5821));
#1094=EDGE_LOOP('',(#5822,#5823,#5824,#5825,#5826,#5827,#5828,#5829,#5830,
#5831,#5832));
#1095=EDGE_LOOP('',(#5833,#5834,#5835,#5836));
#1096=EDGE_LOOP('',(#5837,#5838,#5839,#5840));
#1097=EDGE_LOOP('',(#5841,#5842,#5843,#5844));
#1098=EDGE_LOOP('',(#5845,#5846,#5847,#5848));
#1099=EDGE_LOOP('',(#5849,#5850,#5851,#5852,#5853,#5854,#5855,#5856,#5857,
#5858));
#1100=EDGE_LOOP('',(#5859,#5860,#5861,#5862));
#1101=EDGE_LOOP('',(#5863,#5864,#5865,#5866));
#1102=EDGE_LOOP('',(#5867,#5868,#5869,#5870));
#1103=EDGE_LOOP('',(#5871,#5872,#5873,#5874,#5875,#5876));
#1104=EDGE_LOOP('',(#5877,#5878,#5879,#5880));
#1105=EDGE_LOOP('',(#5881,#5882,#5883,#5884));
#1106=EDGE_LOOP('',(#5885));
#1107=EDGE_LOOP('',(#5886,#5887,#5888,#5889));
#1108=EDGE_LOOP('',(#5890));
#1109=EDGE_LOOP('',(#5891,#5892,#5893,#5894));
#1110=EDGE_LOOP('',(#5895));
#1111=EDGE_LOOP('',(#5896,#5897,#5898,#5899));
#1112=EDGE_LOOP('',(#5900));
#1113=EDGE_LOOP('',(#5901,#5902,#5903,#5904));
#1114=EDGE_LOOP('',(#5905,#5906,#5907,#5908));
#1115=EDGE_LOOP('',(#5909,#5910,#5911,#5912));
#1116=EDGE_LOOP('',(#5913,#5914,#5915,#5916));
#1117=EDGE_LOOP('',(#5917,#5918,#5919,#5920));
#1118=EDGE_LOOP('',(#5921,#5922,#5923,#5924));
#1119=EDGE_LOOP('',(#5925,#5926,#5927,#5928));
#1120=EDGE_LOOP('',(#5929,#5930,#5931,#5932));
#1121=EDGE_LOOP('',(#5933,#5934,#5935,#5936));
#1122=EDGE_LOOP('',(#5937,#5938,#5939,#5940));
#1123=EDGE_LOOP('',(#5941,#5942,#5943,#5944));
#1124=EDGE_LOOP('',(#5945,#5946,#5947,#5948));
#1125=EDGE_LOOP('',(#5949,#5950,#5951,#5952));
#1126=EDGE_LOOP('',(#5953,#5954,#5955,#5956));
#1127=EDGE_LOOP('',(#5957,#5958,#5959,#5960));
#1128=EDGE_LOOP('',(#5961,#5962,#5963,#5964));
#1129=EDGE_LOOP('',(#5965,#5966,#5967,#5968));
#1130=EDGE_LOOP('',(#5969,#5970,#5971,#5972));
#1131=EDGE_LOOP('',(#5973,#5974,#5975,#5976,#5977,#5978,#5979,#5980,#5981,
#5982,#5983,#5984));
#1132=EDGE_LOOP('',(#5985,#5986,#5987,#5988));
#1133=EDGE_LOOP('',(#5989,#5990,#5991,#5992));
#1134=EDGE_LOOP('',(#5993,#5994,#5995,#5996));
#1135=EDGE_LOOP('',(#5997,#5998,#5999,#6000));
#1136=EDGE_LOOP('',(#6001,#6002,#6003,#6004));
#1137=EDGE_LOOP('',(#6005,#6006,#6007,#6008));
#1138=EDGE_LOOP('',(#6009,#6010,#6011,#6012));
#1139=EDGE_LOOP('',(#6013,#6014,#6015,#6016));
#1140=EDGE_LOOP('',(#6017,#6018,#6019,#6020,#6021,#6022,#6023,#6024));
#1141=EDGE_LOOP('',(#6025,#6026,#6027,#6028,#6029,#6030,#6031,#6032));
#1142=EDGE_LOOP('',(#6033,#6034,#6035,#6036));
#1143=EDGE_LOOP('',(#6037,#6038,#6039,#6040));
#1144=EDGE_LOOP('',(#6041,#6042,#6043,#6044));
#1145=EDGE_LOOP('',(#6045));
#1146=EDGE_LOOP('',(#6046));
#1147=EDGE_LOOP('',(#6047,#6048,#6049,#6050));
#1148=EDGE_LOOP('',(#6051,#6052,#6053,#6054));
#1149=EDGE_LOOP('',(#6055,#6056,#6057,#6058));
#1150=EDGE_LOOP('',(#6059,#6060,#6061,#6062));
#1151=EDGE_LOOP('',(#6063));
#1152=EDGE_LOOP('',(#6064));
#1153=EDGE_LOOP('',(#6065,#6066,#6067,#6068));
#1154=EDGE_LOOP('',(#6069,#6070,#6071,#6072));
#1155=EDGE_LOOP('',(#6073,#6074,#6075,#6076));
#1156=EDGE_LOOP('',(#6077,#6078,#6079,#6080));
#1157=EDGE_LOOP('',(#6081));
#1158=EDGE_LOOP('',(#6082));
#1159=EDGE_LOOP('',(#6083,#6084,#6085,#6086));
#1160=EDGE_LOOP('',(#6087,#6088,#6089,#6090));
#1161=EDGE_LOOP('',(#6091,#6092,#6093,#6094));
#1162=EDGE_LOOP('',(#6095,#6096,#6097,#6098));
#1163=EDGE_LOOP('',(#6099));
#1164=EDGE_LOOP('',(#6100));
#1165=EDGE_LOOP('',(#6101,#6102,#6103,#6104));
#1166=EDGE_LOOP('',(#6105,#6106,#6107,#6108,#6109,#6110,#6111,#6112));
#1167=EDGE_LOOP('',(#6113,#6114,#6115,#6116,#6117,#6118,#6119,#6120));
#1168=EDGE_LOOP('',(#6121,#6122,#6123,#6124));
#1169=EDGE_LOOP('',(#6125,#6126,#6127,#6128));
#1170=EDGE_LOOP('',(#6129,#6130,#6131));
#1171=EDGE_LOOP('',(#6132,#6133,#6134,#6135));
#1172=EDGE_LOOP('',(#6136,#6137,#6138));
#1173=EDGE_LOOP('',(#6139,#6140,#6141,#6142));
#1174=EDGE_LOOP('',(#6143,#6144,#6145));
#1175=EDGE_LOOP('',(#6146,#6147,#6148));
#1176=EDGE_LOOP('',(#6149,#6150,#6151,#6152));
#1177=EDGE_LOOP('',(#6153,#6154,#6155,#6156));
#1178=EDGE_LOOP('',(#6157,#6158,#6159,#6160));
#1179=EDGE_LOOP('',(#6161,#6162,#6163,#6164));
#1180=EDGE_LOOP('',(#6165,#6166,#6167,#6168));
#1181=EDGE_LOOP('',(#6169));
#1182=EDGE_LOOP('',(#6170,#6171,#6172));
#1183=EDGE_LOOP('',(#6173,#6174,#6175,#6176));
#1184=EDGE_LOOP('',(#6177,#6178,#6179,#6180));
#1185=EDGE_LOOP('',(#6181,#6182,#6183,#6184));
#1186=EDGE_LOOP('',(#6185,#6186,#6187,#6188));
#1187=EDGE_LOOP('',(#6189,#6190,#6191,#6192));
#1188=EDGE_LOOP('',(#6193,#6194,#6195));
#1189=EDGE_LOOP('',(#6196,#6197,#6198,#6199));
#1190=EDGE_LOOP('',(#6200,#6201,#6202,#6203));
#1191=EDGE_LOOP('',(#6204,#6205,#6206,#6207,#6208,#6209));
#1192=EDGE_LOOP('',(#6210,#6211,#6212,#6213));
#1193=EDGE_LOOP('',(#6214,#6215,#6216,#6217));
#1194=EDGE_LOOP('',(#6218,#6219,#6220,#6221));
#1195=EDGE_LOOP('',(#6222,#6223,#6224,#6225,#6226));
#1196=EDGE_LOOP('',(#6227,#6228,#6229));
#1197=EDGE_LOOP('',(#6230,#6231,#6232,#6233));
#1198=EDGE_LOOP('',(#6234,#6235,#6236,#6237));
#1199=EDGE_LOOP('',(#6238,#6239,#6240,#6241));
#1200=EDGE_LOOP('',(#6242,#6243,#6244,#6245));
#1201=EDGE_LOOP('',(#6246,#6247,#6248,#6249));
#1202=EDGE_LOOP('',(#6250,#6251,#6252));
#1203=EDGE_LOOP('',(#6253,#6254,#6255,#6256));
#1204=EDGE_LOOP('',(#6257,#6258,#6259,#6260));
#1205=EDGE_LOOP('',(#6261,#6262,#6263,#6264,#6265,#6266));
#1206=EDGE_LOOP('',(#6267,#6268,#6269,#6270));
#1207=EDGE_LOOP('',(#6271,#6272,#6273,#6274));
#1208=EDGE_LOOP('',(#6275,#6276,#6277,#6278));
#1209=EDGE_LOOP('',(#6279,#6280,#6281,#6282));
#1210=EDGE_LOOP('',(#6283,#6284,#6285,#6286));
#1211=EDGE_LOOP('',(#6287,#6288,#6289,#6290));
#1212=EDGE_LOOP('',(#6291,#6292,#6293,#6294));
#1213=EDGE_LOOP('',(#6295,#6296,#6297,#6298));
#1214=EDGE_LOOP('',(#6299,#6300,#6301,#6302));
#1215=EDGE_LOOP('',(#6303,#6304,#6305,#6306,#6307,#6308,#6309,#6310,#6311,
#6312,#6313,#6314,#6315,#6316,#6317,#6318));
#1216=EDGE_LOOP('',(#6319,#6320,#6321,#6322,#6323,#6324));
#1217=EDGE_LOOP('',(#6325,#6326,#6327,#6328));
#1218=EDGE_LOOP('',(#6329,#6330,#6331,#6332));
#1219=EDGE_LOOP('',(#6333,#6334,#6335,#6336));
#1220=EDGE_LOOP('',(#6337,#6338,#6339,#6340));
#1221=EDGE_LOOP('',(#6341,#6342,#6343,#6344));
#1222=EDGE_LOOP('',(#6345,#6346,#6347,#6348,#6349,#6350));
#1223=EDGE_LOOP('',(#6351,#6352,#6353,#6354));
#1224=EDGE_LOOP('',(#6355,#6356,#6357,#6358));
#1225=EDGE_LOOP('',(#6359,#6360,#6361,#6362));
#1226=EDGE_LOOP('',(#6363,#6364,#6365,#6366));
#1227=EDGE_LOOP('',(#6367,#6368,#6369,#6370,#6371,#6372,#6373,#6374,#6375,
#6376,#6377,#6378));
#1228=EDGE_LOOP('',(#6379,#6380));
#1229=EDGE_LOOP('',(#6381,#6382,#6383,#6384));
#1230=EDGE_LOOP('',(#6385,#6386,#6387,#6388));
#1231=EDGE_LOOP('',(#6389,#6390,#6391,#6392));
#1232=EDGE_LOOP('',(#6393,#6394,#6395,#6396));
#1233=EDGE_LOOP('',(#6397,#6398,#6399,#6400));
#1234=EDGE_LOOP('',(#6401,#6402,#6403,#6404));
#1235=EDGE_LOOP('',(#6405,#6406,#6407,#6408));
#1236=EDGE_LOOP('',(#6409,#6410,#6411,#6412,#6413,#6414,#6415,#6416,#6417,
#6418,#6419,#6420));
#1237=EDGE_LOOP('',(#6421,#6422));
#1238=EDGE_LOOP('',(#6423,#6424,#6425,#6426));
#1239=EDGE_LOOP('',(#6427,#6428,#6429,#6430));
#1240=EDGE_LOOP('',(#6431,#6432,#6433,#6434));
#1241=EDGE_LOOP('',(#6435,#6436,#6437,#6438));
#1242=EDGE_LOOP('',(#6439,#6440,#6441,#6442));
#1243=EDGE_LOOP('',(#6443,#6444,#6445,#6446));
#1244=EDGE_LOOP('',(#6447,#6448,#6449,#6450));
#1245=EDGE_LOOP('',(#6451,#6452,#6453,#6454));
#1246=EDGE_LOOP('',(#6455,#6456,#6457,#6458));
#1247=EDGE_LOOP('',(#6459,#6460));
#1248=EDGE_LOOP('',(#6461,#6462,#6463,#6464));
#1249=EDGE_LOOP('',(#6465,#6466));
#1250=EDGE_LOOP('',(#6467,#6468,#6469,#6470));
#1251=EDGE_LOOP('',(#6471,#6472,#6473,#6474));
#1252=EDGE_LOOP('',(#6475,#6476,#6477,#6478));
#1253=EDGE_LOOP('',(#6479,#6480,#6481,#6482));
#1254=EDGE_LOOP('',(#6483,#6484,#6485,#6486));
#1255=EDGE_LOOP('',(#6487,#6488,#6489,#6490));
#1256=EDGE_LOOP('',(#6491,#6492,#6493,#6494));
#1257=EDGE_LOOP('',(#6495,#6496,#6497,#6498));
#1258=EDGE_LOOP('',(#6499,#6500,#6501,#6502));
#1259=EDGE_LOOP('',(#6503,#6504,#6505,#6506,#6507,#6508,#6509,#6510));
#1260=EDGE_LOOP('',(#6511,#6512,#6513,#6514,#6515,#6516,#6517,#6518));
#1261=EDGE_LOOP('',(#6519,#6520,#6521,#6522));
#1262=EDGE_LOOP('',(#6523,#6524,#6525,#6526));
#1263=EDGE_LOOP('',(#6527));
#1264=EDGE_LOOP('',(#6528));
#1265=EDGE_LOOP('',(#6529,#6530,#6531,#6532));
#1266=EDGE_LOOP('',(#6533));
#1267=EDGE_LOOP('',(#6534));
#1268=EDGE_LOOP('',(#6535,#6536,#6537,#6538));
#1269=EDGE_LOOP('',(#6539,#6540,#6541,#6542));
#1270=EDGE_LOOP('',(#6543,#6544,#6545,#6546));
#1271=EDGE_LOOP('',(#6547,#6548,#6549,#6550));
#1272=EDGE_LOOP('',(#6551,#6552,#6553,#6554));
#1273=EDGE_LOOP('',(#6555,#6556,#6557,#6558));
#1274=EDGE_LOOP('',(#6559,#6560,#6561,#6562));
#1275=EDGE_LOOP('',(#6563,#6564,#6565,#6566));
#1276=EDGE_LOOP('',(#6567,#6568,#6569,#6570));
#1277=EDGE_LOOP('',(#6571,#6572,#6573,#6574,#6575));
#1278=EDGE_LOOP('',(#6576,#6577,#6578,#6579));
#1279=EDGE_LOOP('',(#6580,#6581,#6582,#6583));
#1280=EDGE_LOOP('',(#6584,#6585,#6586,#6587,#6588,#6589));
#1281=EDGE_LOOP('',(#6590));
#1282=EDGE_LOOP('',(#6591,#6592));
#1283=EDGE_LOOP('',(#6593,#6594,#6595,#6596));
#1284=EDGE_LOOP('',(#6597,#6598,#6599,#6600));
#1285=EDGE_LOOP('',(#6601,#6602,#6603,#6604));
#1286=EDGE_LOOP('',(#6605,#6606,#6607,#6608));
#1287=EDGE_LOOP('',(#6609,#6610,#6611,#6612));
#1288=EDGE_LOOP('',(#6613,#6614,#6615,#6616));
#1289=EDGE_LOOP('',(#6617,#6618,#6619,#6620));
#1290=EDGE_LOOP('',(#6621,#6622,#6623,#6624));
#1291=EDGE_LOOP('',(#6625,#6626,#6627,#6628));
#1292=EDGE_LOOP('',(#6629,#6630,#6631,#6632,#6633,#6634,#6635,#6636,#6637,
#6638,#6639,#6640,#6641,#6642,#6643,#6644));
#1293=EDGE_LOOP('',(#6645,#6646,#6647,#6648,#6649,#6650));
#1294=EDGE_LOOP('',(#6651));
#1295=EDGE_LOOP('',(#6652,#6653));
#1296=EDGE_LOOP('',(#6654,#6655,#6656,#6657));
#1297=EDGE_LOOP('',(#6658,#6659,#6660,#6661));
#1298=EDGE_LOOP('',(#6662));
#1299=EDGE_LOOP('',(#6663));
#1300=EDGE_LOOP('',(#6664,#6665,#6666,#6667));
#1301=EDGE_LOOP('',(#6668,#6669,#6670,#6671,#6672));
#1302=EDGE_LOOP('',(#6673,#6674,#6675,#6676,#6677));
#1303=EDGE_LOOP('',(#6678));
#1304=EDGE_LOOP('',(#6679));
#1305=EDGE_LOOP('',(#6680,#6681,#6682,#6683));
#1306=EDGE_LOOP('',(#6684,#6685,#6686,#6687));
#1307=EDGE_LOOP('',(#6688,#6689,#6690,#6691));
#1308=EDGE_LOOP('',(#6692));
#1309=EDGE_LOOP('',(#6693,#6694,#6695,#6696));
#1310=EDGE_LOOP('',(#6697,#6698,#6699,#6700));
#1311=EDGE_LOOP('',(#6701,#6702,#6703,#6704));
#1312=EDGE_LOOP('',(#6705,#6706,#6707,#6708));
#1313=EDGE_LOOP('',(#6709,#6710,#6711,#6712));
#1314=EDGE_LOOP('',(#6713,#6714,#6715,#6716));
#1315=EDGE_LOOP('',(#6717,#6718,#6719,#6720));
#1316=EDGE_LOOP('',(#6721,#6722,#6723,#6724));
#1317=EDGE_LOOP('',(#6725,#6726,#6727,#6728));
#1318=EDGE_LOOP('',(#6729,#6730,#6731,#6732));
#1319=EDGE_LOOP('',(#6733,#6734,#6735,#6736));
#1320=EDGE_LOOP('',(#6737,#6738,#6739,#6740,#6741,#6742,#6743,#6744,#6745,
#6746,#6747,#6748,#6749,#6750,#6751));
#1321=EDGE_LOOP('',(#6752,#6753,#6754,#6755));
#1322=EDGE_LOOP('',(#6756,#6757,#6758,#6759,#6760,#6761,#6762,#6763,#6764,
#6765,#6766,#6767,#6768,#6769,#6770));
#1323=EDGE_LOOP('',(#6771));
#1324=EDGE_LOOP('',(#6772,#6773,#6774,#6775));
#1325=EDGE_LOOP('',(#6776,#6777,#6778,#6779));
#1326=EDGE_LOOP('',(#6780));
#1327=EDGE_LOOP('',(#6781));
#1328=EDGE_LOOP('',(#6782,#6783,#6784,#6785));
#1329=EDGE_LOOP('',(#6786));
#1330=EDGE_LOOP('',(#6787,#6788,#6789,#6790));
#1331=EDGE_LOOP('',(#6791,#6792,#6793,#6794));
#1332=EDGE_LOOP('',(#6795,#6796,#6797));
#1333=EDGE_LOOP('',(#6798,#6799,#6800));
#1334=EDGE_LOOP('',(#6801,#6802,#6803));
#1335=EDGE_LOOP('',(#6804,#6805,#6806));
#1336=EDGE_LOOP('',(#6807,#6808,#6809,#6810));
#1337=EDGE_LOOP('',(#6811,#6812,#6813,#6814));
#1338=EDGE_LOOP('',(#6815,#6816,#6817,#6818));
#1339=EDGE_LOOP('',(#6819,#6820,#6821,#6822));
#1340=EDGE_LOOP('',(#6823,#6824,#6825,#6826));
#1341=EDGE_LOOP('',(#6827,#6828,#6829,#6830));
#1342=EDGE_LOOP('',(#6831,#6832,#6833,#6834));
#1343=EDGE_LOOP('',(#6835,#6836,#6837,#6838));
#1344=EDGE_LOOP('',(#6839,#6840,#6841,#6842));
#1345=EDGE_LOOP('',(#6843,#6844,#6845,#6846));
#1346=EDGE_LOOP('',(#6847,#6848,#6849,#6850));
#1347=EDGE_LOOP('',(#6851,#6852,#6853,#6854));
#1348=EDGE_LOOP('',(#6855,#6856,#6857,#6858));
#1349=EDGE_LOOP('',(#6859,#6860,#6861,#6862));
#1350=EDGE_LOOP('',(#6863,#6864,#6865,#6866));
#1351=EDGE_LOOP('',(#6867,#6868,#6869,#6870));
#1352=EDGE_LOOP('',(#6871,#6872,#6873,#6874));
#1353=EDGE_LOOP('',(#6875,#6876,#6877,#6878));
#1354=EDGE_LOOP('',(#6879,#6880,#6881,#6882,#6883,#6884,#6885,#6886));
#1355=EDGE_LOOP('',(#6887,#6888,#6889,#6890));
#1356=EDGE_LOOP('',(#6891,#6892,#6893,#6894,#6895,#6896,#6897,#6898));
#1357=EDGE_LOOP('',(#6899,#6900,#6901,#6902,#6903,#6904,#6905,#6906));
#1358=EDGE_LOOP('',(#6907,#6908,#6909,#6910));
#1359=EDGE_LOOP('',(#6911,#6912,#6913,#6914));
#1360=EDGE_LOOP('',(#6915,#6916,#6917,#6918));
#1361=EDGE_LOOP('',(#6919,#6920,#6921,#6922));
#1362=EDGE_LOOP('',(#6923,#6924,#6925,#6926));
#1363=EDGE_LOOP('',(#6927,#6928,#6929,#6930));
#1364=EDGE_LOOP('',(#6931,#6932,#6933,#6934));
#1365=EDGE_LOOP('',(#6935,#6936,#6937,#6938));
#1366=EDGE_LOOP('',(#6939,#6940,#6941,#6942,#6943,#6944));
#1367=EDGE_LOOP('',(#6945,#6946,#6947));
#1368=EDGE_LOOP('',(#6948,#6949,#6950,#6951,#6952,#6953));
#1369=EDGE_LOOP('',(#6954,#6955,#6956));
#1370=EDGE_LOOP('',(#6957,#6958,#6959,#6960,#6961,#6962));
#1371=EDGE_LOOP('',(#6963,#6964,#6965));
#1372=EDGE_LOOP('',(#6966,#6967,#6968,#6969,#6970,#6971));
#1373=EDGE_LOOP('',(#6972,#6973,#6974));
#1374=EDGE_LOOP('',(#6975,#6976,#6977,#6978,#6979,#6980));
#1375=EDGE_LOOP('',(#6981,#6982,#6983));
#1376=EDGE_LOOP('',(#6984,#6985,#6986,#6987,#6988,#6989));
#1377=EDGE_LOOP('',(#6990,#6991,#6992));
#1378=EDGE_LOOP('',(#6993,#6994,#6995));
#1379=EDGE_LOOP('',(#6996,#6997,#6998,#6999,#7000,#7001,#7002));
#1380=EDGE_LOOP('',(#7003,#7004,#7005));
#1381=EDGE_LOOP('',(#7006,#7007,#7008,#7009,#7010,#7011));
#1382=EDGE_LOOP('',(#7012,#7013,#7014,#7015,#7016,#7017,#7018,#7019));
#1383=EDGE_LOOP('',(#7020,#7021,#7022,#7023));
#1384=EDGE_LOOP('',(#7024));
#1385=EDGE_LOOP('',(#7025));
#1386=EDGE_LOOP('',(#7026,#7027,#7028,#7029));
#1387=EDGE_LOOP('',(#7030,#7031,#7032,#7033));
#1388=EDGE_LOOP('',(#7034,#7035,#7036,#7037));
#1389=EDGE_LOOP('',(#7038));
#1390=EDGE_LOOP('',(#7039,#7040,#7041,#7042,#7043,#7044,#7045,#7046,#7047,
#7048,#7049,#7050,#7051,#7052,#7053,#7054,#7055,#7056,#7057,#7058,#7059));
#1391=EDGE_LOOP('',(#7060,#7061,#7062,#7063,#7064));
#1392=EDGE_LOOP('',(#7065,#7066,#7067,#7068,#7069,#7070));
#1393=EDGE_LOOP('',(#7071,#7072,#7073));
#1394=EDGE_LOOP('',(#7074,#7075,#7076,#7077,#7078,#7079));
#1395=EDGE_LOOP('',(#7080,#7081,#7082));
#1396=EDGE_LOOP('',(#7083,#7084,#7085,#7086,#7087,#7088));
#1397=EDGE_LOOP('',(#7089,#7090,#7091));
#1398=EDGE_LOOP('',(#7092,#7093,#7094,#7095,#7096,#7097));
#1399=EDGE_LOOP('',(#7098,#7099,#7100));
#1400=EDGE_LOOP('',(#7101,#7102,#7103,#7104,#7105,#7106));
#1401=EDGE_LOOP('',(#7107,#7108,#7109));
#1402=EDGE_LOOP('',(#7110,#7111,#7112,#7113,#7114,#7115));
#1403=EDGE_LOOP('',(#7116,#7117,#7118));
#1404=EDGE_LOOP('',(#7119,#7120,#7121));
#1405=EDGE_LOOP('',(#7122,#7123,#7124,#7125,#7126,#7127,#7128));
#1406=EDGE_LOOP('',(#7129,#7130,#7131));
#1407=EDGE_LOOP('',(#7132,#7133,#7134,#7135,#7136,#7137));
#1408=EDGE_LOOP('',(#7138,#7139,#7140,#7141,#7142,#7143,#7144,#7145));
#1409=EDGE_LOOP('',(#7146,#7147,#7148,#7149));
#1410=EDGE_LOOP('',(#7150));
#1411=EDGE_LOOP('',(#7151));
#1412=EDGE_LOOP('',(#7152,#7153,#7154,#7155));
#1413=EDGE_LOOP('',(#7156,#7157,#7158,#7159));
#1414=EDGE_LOOP('',(#7160,#7161,#7162,#7163));
#1415=EDGE_LOOP('',(#7164));
#1416=EDGE_LOOP('',(#7165,#7166,#7167,#7168,#7169,#7170,#7171,#7172,#7173,
#7174,#7175,#7176,#7177,#7178,#7179,#7180,#7181,#7182,#7183,#7184,#7185));
#1417=EDGE_LOOP('',(#7186,#7187,#7188,#7189,#7190));
#1418=EDGE_LOOP('',(#7191,#7192,#7193,#7194,#7195,#7196));
#1419=EDGE_LOOP('',(#7197,#7198,#7199));
#1420=EDGE_LOOP('',(#7200,#7201,#7202,#7203,#7204,#7205));
#1421=EDGE_LOOP('',(#7206,#7207,#7208));
#1422=EDGE_LOOP('',(#7209,#7210,#7211,#7212,#7213,#7214));
#1423=EDGE_LOOP('',(#7215,#7216,#7217));
#1424=EDGE_LOOP('',(#7218,#7219,#7220,#7221,#7222,#7223));
#1425=EDGE_LOOP('',(#7224,#7225,#7226));
#1426=EDGE_LOOP('',(#7227,#7228,#7229,#7230,#7231,#7232));
#1427=EDGE_LOOP('',(#7233,#7234,#7235));
#1428=EDGE_LOOP('',(#7236,#7237,#7238,#7239,#7240,#7241));
#1429=EDGE_LOOP('',(#7242,#7243,#7244));
#1430=EDGE_LOOP('',(#7245,#7246,#7247));
#1431=EDGE_LOOP('',(#7248,#7249,#7250,#7251,#7252,#7253,#7254));
#1432=EDGE_LOOP('',(#7255,#7256,#7257));
#1433=EDGE_LOOP('',(#7258,#7259,#7260,#7261,#7262,#7263));
#1434=EDGE_LOOP('',(#7264,#7265,#7266,#7267,#7268,#7269,#7270,#7271));
#1435=EDGE_LOOP('',(#7272,#7273,#7274,#7275));
#1436=EDGE_LOOP('',(#7276));
#1437=EDGE_LOOP('',(#7277));
#1438=EDGE_LOOP('',(#7278,#7279,#7280,#7281));
#1439=EDGE_LOOP('',(#7282,#7283,#7284,#7285));
#1440=EDGE_LOOP('',(#7286,#7287,#7288,#7289));
#1441=EDGE_LOOP('',(#7290));
#1442=EDGE_LOOP('',(#7291,#7292,#7293,#7294,#7295,#7296,#7297,#7298,#7299,
#7300,#7301,#7302,#7303,#7304,#7305,#7306,#7307,#7308,#7309,#7310,#7311));
#1443=EDGE_LOOP('',(#7312,#7313,#7314,#7315,#7316));
#1444=EDGE_LOOP('',(#7317,#7318,#7319,#7320,#7321,#7322));
#1445=EDGE_LOOP('',(#7323,#7324,#7325));
#1446=EDGE_LOOP('',(#7326,#7327,#7328,#7329,#7330,#7331));
#1447=EDGE_LOOP('',(#7332,#7333,#7334));
#1448=EDGE_LOOP('',(#7335,#7336,#7337,#7338,#7339,#7340));
#1449=EDGE_LOOP('',(#7341,#7342,#7343));
#1450=EDGE_LOOP('',(#7344,#7345,#7346,#7347,#7348,#7349));
#1451=EDGE_LOOP('',(#7350,#7351,#7352));
#1452=EDGE_LOOP('',(#7353,#7354,#7355,#7356,#7357,#7358));
#1453=EDGE_LOOP('',(#7359,#7360,#7361));
#1454=EDGE_LOOP('',(#7362,#7363,#7364,#7365,#7366,#7367));
#1455=EDGE_LOOP('',(#7368,#7369,#7370));
#1456=EDGE_LOOP('',(#7371,#7372,#7373));
#1457=EDGE_LOOP('',(#7374,#7375,#7376,#7377,#7378,#7379,#7380));
#1458=EDGE_LOOP('',(#7381,#7382,#7383));
#1459=EDGE_LOOP('',(#7384,#7385,#7386,#7387,#7388,#7389));
#1460=EDGE_LOOP('',(#7390,#7391,#7392,#7393,#7394,#7395,#7396,#7397));
#1461=EDGE_LOOP('',(#7398,#7399,#7400,#7401));
#1462=EDGE_LOOP('',(#7402));
#1463=EDGE_LOOP('',(#7403));
#1464=EDGE_LOOP('',(#7404,#7405,#7406,#7407));
#1465=EDGE_LOOP('',(#7408,#7409,#7410,#7411));
#1466=EDGE_LOOP('',(#7412,#7413,#7414,#7415));
#1467=EDGE_LOOP('',(#7416));
#1468=EDGE_LOOP('',(#7417,#7418,#7419,#7420,#7421,#7422,#7423,#7424,#7425,
#7426,#7427,#7428,#7429,#7430,#7431,#7432,#7433,#7434,#7435,#7436,#7437));
#1469=EDGE_LOOP('',(#7438,#7439,#7440,#7441,#7442));
#1470=CIRCLE('',#8263,4.5);
#1471=CIRCLE('',#8264,4.5);
#1472=CIRCLE('',#8265,4.5);
#1473=CIRCLE('',#8269,1.);
#1474=CIRCLE('',#8272,0.999999999999998);
#1475=CIRCLE('',#8273,0.999999999999998);
#1476=CIRCLE('',#8278,2.);
#1477=CIRCLE('',#8279,2.);
#1478=CIRCLE('',#8280,1.5);
#1479=CIRCLE('',#8281,1.5);
#1480=CIRCLE('',#8282,1.5);
#1481=CIRCLE('',#8283,1.5);
#1482=CIRCLE('',#8285,0.999999999999999);
#1483=CIRCLE('',#8286,1.);
#1484=CIRCLE('',#8288,1.);
#1485=CIRCLE('',#8293,1.);
#1486=CIRCLE('',#8294,0.999999999999999);
#1487=CIRCLE('',#8296,1.);
#1488=CIRCLE('',#8297,3.5);
#1489=CIRCLE('',#8298,2.5);
#1490=CIRCLE('',#8301,1.);
#1491=CIRCLE('',#8302,3.5);
#1492=CIRCLE('',#8303,2.5);
#1493=CIRCLE('',#8305,0.999999999999999);
#1494=CIRCLE('',#8307,1.);
#1495=CIRCLE('',#8309,1.);
#1496=CIRCLE('',#8310,1.);
#1497=CIRCLE('',#8312,1.);
#1498=CIRCLE('',#8315,1.);
#1499=CIRCLE('',#8317,3.5);
#1500=CIRCLE('',#8318,2.);
#1501=CIRCLE('',#8319,1.);
#1502=CIRCLE('',#8320,1.);
#1503=CIRCLE('',#8321,3.5);
#1504=CIRCLE('',#8323,1.);
#1505=CIRCLE('',#8328,2.);
#1506=CIRCLE('',#8329,2.);
#1507=CIRCLE('',#8332,2.);
#1508=CIRCLE('',#8333,2.);
#1509=CIRCLE('',#8336,1.5);
#1510=CIRCLE('',#8337,1.5);
#1511=CIRCLE('',#8338,3.);
#1512=CIRCLE('',#8339,2.);
#1513=CIRCLE('',#8340,0.999999999999996);
#1514=CIRCLE('',#8341,2.);
#1515=CIRCLE('',#8342,2.);
#1516=CIRCLE('',#8344,1.5);
#1517=CIRCLE('',#8345,1.5);
#1518=CIRCLE('',#8346,1.5);
#1519=CIRCLE('',#8348,1.5);
#1520=CIRCLE('',#8349,1.5);
#1521=CIRCLE('',#8350,1.5);
#1522=CIRCLE('',#8352,1.5);
#1523=CIRCLE('',#8353,1.5);
#1524=CIRCLE('',#8355,1.5);
#1525=CIRCLE('',#8356,1.5);
#1526=CIRCLE('',#8360,4.5);
#1527=CIRCLE('',#8366,4.5);
#1528=CIRCLE('',#8367,4.5);
#1529=CIRCLE('',#8368,4.5);
#1530=CIRCLE('',#8369,3.);
#1531=CIRCLE('',#8372,3.);
#1532=CIRCLE('',#8374,4.5);
#1533=CIRCLE('',#8383,4.5);
#1534=CIRCLE('',#8387,1.);
#1535=CIRCLE('',#8388,0.999999999999996);
#1536=CIRCLE('',#8390,0.999999999999996);
#1537=CIRCLE('',#8391,2.5);
#1538=CIRCLE('',#8393,0.999999999999996);
#1539=CIRCLE('',#8395,1.);
#1540=CIRCLE('',#8396,0.999999999999996);
#1541=CIRCLE('',#8397,1.);
#1542=CIRCLE('',#8399,1.);
#1543=CIRCLE('',#8400,1.00000000000001);
#1544=CIRCLE('',#8401,2.);
#1545=CIRCLE('',#8403,0.999999999999996);
#1546=CIRCLE('',#8404,1.);
#1547=CIRCLE('',#8405,2.);
#1548=CIRCLE('',#8407,1.);
#1549=CIRCLE('',#8409,1.);
#1550=CIRCLE('',#8410,0.999999999999996);
#1551=CIRCLE('',#8412,1.);
#1552=CIRCLE('',#8413,2.5);
#1553=CIRCLE('',#8415,0.999999999999998);
#1554=CIRCLE('',#8417,1.);
#1555=CIRCLE('',#8419,1.);
#1556=CIRCLE('',#8421,1.);
#1557=CIRCLE('',#8423,1.);
#1558=CIRCLE('',#8426,2.5);
#1559=CIRCLE('',#8429,1.);
#1560=CIRCLE('',#8434,0.999999999999996);
#1561=CIRCLE('',#8436,1.);
#1562=CIRCLE('',#8438,2.5);
#1563=CIRCLE('',#8441,1.);
#1564=CIRCLE('',#8445,2.5);
#1565=CIRCLE('',#8447,2.);
#1566=CIRCLE('',#8449,2.);
#1567=CIRCLE('',#8452,2.5);
#1568=CIRCLE('',#8455,2.);
#1569=CIRCLE('',#8464,2.);
#1570=CIRCLE('',#8465,1.99999999999999);
#1571=CIRCLE('',#8466,0.999999999999996);
#1572=CIRCLE('',#8467,2.00000000000001);
#1573=CIRCLE('',#8468,3.);
#1574=CIRCLE('',#8469,3.5);
#1575=CIRCLE('',#8470,3.5);
#1576=CIRCLE('',#8471,1.5);
#1577=CIRCLE('',#8472,1.5);
#1578=CIRCLE('',#8473,1.);
#1579=CIRCLE('',#8474,2.);
#1580=CIRCLE('',#8475,1.);
#1581=CIRCLE('',#8476,1.);
#1582=CIRCLE('',#8478,1.);
#1583=CIRCLE('',#8479,1.);
#1584=CIRCLE('',#8480,2.);
#1585=CIRCLE('',#8481,1.);
#1586=CIRCLE('',#8482,1.);
#1587=CIRCLE('',#8486,1.);
#1588=CIRCLE('',#8487,2.);
#1589=CIRCLE('',#8488,1.);
#1590=CIRCLE('',#8490,2.);
#1591=CIRCLE('',#8493,2.);
#1592=CIRCLE('',#8495,4.);
#1593=CIRCLE('',#8499,2.);
#1594=CIRCLE('',#8502,0.999999999999999);
#1595=CIRCLE('',#8503,1.);
#1596=CIRCLE('',#8505,4.);
#1597=CIRCLE('',#8510,0.999999999999999);
#1598=CIRCLE('',#8512,1.);
#1599=CIRCLE('',#8514,3.5);
#1600=CIRCLE('',#8515,3.5);
#1601=CIRCLE('',#8516,2.);
#1602=CIRCLE('',#8517,2.);
#1603=CIRCLE('',#8518,1.5);
#1604=CIRCLE('',#8519,1.5);
#1605=CIRCLE('',#8521,2.);
#1606=CIRCLE('',#8522,2.);
#1607=CIRCLE('',#8526,2.);
#1608=CIRCLE('',#8527,2.);
#1609=CIRCLE('',#8532,3.5);
#1610=CIRCLE('',#8533,3.5);
#1611=CIRCLE('',#8534,3.);
#1612=CIRCLE('',#8535,3.5);
#1613=CIRCLE('',#8536,3.5);
#1614=CIRCLE('',#8548,1.5);
#1615=CIRCLE('',#8551,1.5);
#1616=CIRCLE('',#8554,1.5);
#1617=CIRCLE('',#8557,1.5);
#1618=CIRCLE('',#8560,1.);
#1619=CIRCLE('',#8561,1.);
#1620=CIRCLE('',#8563,0.999999999999996);
#1621=CIRCLE('',#8564,2.);
#1622=CIRCLE('',#8565,0.999999999999996);
#1623=CIRCLE('',#8567,0.999999999999996);
#1624=CIRCLE('',#8568,1.);
#1625=CIRCLE('',#8569,0.999999999999993);
#1626=CIRCLE('',#8570,1.99999999999999);
#1627=CIRCLE('',#8572,1.);
#1628=CIRCLE('',#8573,1.);
#1629=CIRCLE('',#8574,0.999999999999997);
#1630=CIRCLE('',#8575,2.);
#1631=CIRCLE('',#8577,1.);
#1632=CIRCLE('',#8578,0.999999999999999);
#1633=CIRCLE('',#8579,0.999999999999998);
#1634=CIRCLE('',#8580,2.);
#1635=CIRCLE('',#8582,0.999999999999999);
#1636=CIRCLE('',#8583,0.999999999999996);
#1637=CIRCLE('',#8584,1.);
#1638=CIRCLE('',#8585,2.);
#1639=CIRCLE('',#8587,0.999999999999996);
#1640=CIRCLE('',#8588,1.00000000000001);
#1641=CIRCLE('',#8589,2.00000000000001);
#1642=CIRCLE('',#8603,3.20000000000001);
#1643=CIRCLE('',#8604,3.20000000000001);
#1644=CIRCLE('',#8606,3.20000000000001);
#1645=CIRCLE('',#8607,3.20000000000001);
#1646=CIRCLE('',#8609,3.2);
#1647=CIRCLE('',#8610,3.2);
#1648=CIRCLE('',#8612,3.2);
#1649=CIRCLE('',#8613,3.2);
#1650=CIRCLE('',#8615,2.);
#1651=CIRCLE('',#8616,2.);
#1652=CIRCLE('',#8617,2.);
#1653=CIRCLE('',#8618,2.);
#1654=CIRCLE('',#8619,0.999999999999999);
#1655=CIRCLE('',#8620,0.999999999999999);
#1656=CIRCLE('',#8621,0.999999999999999);
#1657=CIRCLE('',#8622,1.);
#1658=CIRCLE('',#8625,0.999999999999999);
#1659=CIRCLE('',#8628,0.999999999999999);
#1660=CIRCLE('',#8631,1.);
#1661=CIRCLE('',#8634,0.999999999999999);
#1662=CIRCLE('',#8637,2.);
#1663=CIRCLE('',#8640,2.);
#1664=CIRCLE('',#8643,2.);
#1665=CIRCLE('',#8646,2.);
#1666=CIRCLE('',#8650,1.99999999999996);
#1667=CIRCLE('',#8651,2.);
#1668=CIRCLE('',#8653,1.99999999999996);
#1669=CIRCLE('',#8654,2.);
#1670=CIRCLE('',#8656,2.);
#1671=CIRCLE('',#8658,1.99999999999996);
#1672=CIRCLE('',#8659,2.);
#1673=CIRCLE('',#8661,2.);
#1674=CIRCLE('',#8663,1.99999999999996);
#1675=CIRCLE('',#8664,2.);
#1676=CIRCLE('',#8666,2.);
#1677=CIRCLE('',#8668,2.00000000000001);
#1678=CIRCLE('',#8670,2.);
#1679=CIRCLE('',#8673,2.00000000000001);
#1680=CIRCLE('',#8676,9.);
#1681=CIRCLE('',#8678,0.200000000000002);
#1682=CIRCLE('',#8679,0.2);
#1683=CIRCLE('',#8680,0.200000000000002);
#1684=CIRCLE('',#8682,0.200000000000008);
#1685=CIRCLE('',#8683,0.199999999999995);
#1686=CIRCLE('',#8684,0.199999999999991);
#1687=CIRCLE('',#8687,0.2);
#1688=CIRCLE('',#8689,0.200000000000012);
#1689=CIRCLE('',#8691,0.200000000000002);
#1690=CIRCLE('',#8692,0.2);
#1691=CIRCLE('',#8695,0.999999999999871);
#1692=CIRCLE('',#8698,0.999999999999871);
#1693=CIRCLE('',#8701,0.2);
#1694=CIRCLE('',#8703,9.);
#1695=CIRCLE('',#8704,9.);
#1696=CIRCLE('',#8705,0.2);
#1697=CIRCLE('',#8706,9.2);
#1698=CIRCLE('',#8708,0.199999999999995);
#1699=CIRCLE('',#8709,0.2);
#1700=CIRCLE('',#8710,0.199999999999995);
#1701=CIRCLE('',#8712,0.200000000000009);
#1702=CIRCLE('',#8713,0.199999999999999);
#1703=CIRCLE('',#8714,0.199999999999995);
#1704=CIRCLE('',#8717,0.2);
#1705=CIRCLE('',#8719,0.200000000000012);
#1706=CIRCLE('',#8721,0.199999999999995);
#1707=CIRCLE('',#8724,0.999999999999871);
#1708=CIRCLE('',#8727,0.999999999999871);
#1709=CIRCLE('',#8730,0.2);
#1710=CIRCLE('',#8732,9.2);
#1711=CIRCLE('',#8733,9.);
#1712=CIRCLE('',#8735,0.2);
#1713=CIRCLE('',#8736,0.2);
#1714=CIRCLE('',#8737,0.2);
#1715=CIRCLE('',#8738,0.4);
#1716=CIRCLE('',#8740,0.2);
#1717=CIRCLE('',#8741,0.2);
#1718=CIRCLE('',#8742,0.4);
#1719=CIRCLE('',#8744,0.4);
#1720=CIRCLE('',#8748,0.2);
#1721=CIRCLE('',#8749,0.2);
#1722=CIRCLE('',#8750,0.2);
#1723=CIRCLE('',#8751,0.4);
#1724=CIRCLE('',#8753,0.2);
#1725=CIRCLE('',#8754,0.2);
#1726=CIRCLE('',#8755,0.4);
#1727=CIRCLE('',#8757,0.4);
#1728=CIRCLE('',#8760,0.4);
#1729=CIRCLE('',#8761,0.399999999999992);
#1730=CIRCLE('',#8763,0.4);
#1731=CIRCLE('',#8764,1.39999999999987);
#1732=CIRCLE('',#8766,0.4);
#1733=CIRCLE('',#8767,0.800000000000059);
#1734=CIRCLE('',#8768,0.400000000000058);
#1735=CIRCLE('',#8770,1.39999999999987);
#1736=CIRCLE('',#8771,0.400000000000058);
#1737=CIRCLE('',#8772,2.98575787723652);
#1738=CIRCLE('',#8774,0.400000000000004);
#1739=CIRCLE('',#8776,0.399999999999992);
#1740=CIRCLE('',#8777,0.399999999999994);
#1741=CIRCLE('',#8778,0.800000000000059);
#1742=CIRCLE('',#8780,0.4);
#1743=CIRCLE('',#8781,0.399999999999991);
#1744=CIRCLE('',#8783,0.4);
#1745=CIRCLE('',#8784,1.39999999999987);
#1746=CIRCLE('',#8786,0.4);
#1747=CIRCLE('',#8787,0.800000000000059);
#1748=CIRCLE('',#8788,0.400000000000058);
#1749=CIRCLE('',#8790,1.39999999999987);
#1750=CIRCLE('',#8791,0.400000000000058);
#1751=CIRCLE('',#8792,2.98575787723652);
#1752=CIRCLE('',#8794,0.400000000000005);
#1753=CIRCLE('',#8796,0.399999999999992);
#1754=CIRCLE('',#8797,0.399999999999994);
#1755=CIRCLE('',#8798,0.800000000000059);
#1756=CIRCLE('',#8804,2.98575787723652);
#1757=CIRCLE('',#8809,2.98575787723652);
#1758=CIRCLE('',#8812,0.399999999999998);
#1759=CIRCLE('',#8814,0.4);
#1760=CIRCLE('',#8816,0.400000000000004);
#1761=CIRCLE('',#8818,0.4);
#1762=CIRCLE('',#8820,2.);
#1763=CIRCLE('',#8823,2.);
#1764=CIRCLE('',#8828,8.);
#1765=CIRCLE('',#8829,7.);
#1766=CIRCLE('',#8831,7.);
#1767=CIRCLE('',#8833,9.);
#1768=CIRCLE('',#8835,8.);
#1769=CIRCLE('',#8837,9.);
#1770=CIRCLE('',#8840,0.400000000000001);
#1771=CIRCLE('',#8841,0.399999999999991);
#1772=CIRCLE('',#8842,0.4);
#1773=CIRCLE('',#8843,0.400000000000001);
#1774=CIRCLE('',#8845,0.400000000000003);
#1775=CIRCLE('',#8846,0.4);
#1776=CIRCLE('',#8848,0.4);
#1777=CIRCLE('',#8849,0.4);
#1778=CIRCLE('',#8853,9.);
#1779=CIRCLE('',#8854,9.);
#1780=CIRCLE('',#8855,8.6);
#1781=CIRCLE('',#8857,6.5);
#1782=CIRCLE('',#8858,6.5);
#1783=CIRCLE('',#8860,9.);
#1784=CIRCLE('',#8862,4.);
#1785=CIRCLE('',#8864,0.4);
#1786=CIRCLE('',#8865,0.400000000000001);
#1787=CIRCLE('',#8866,0.400000000000001);
#1788=CIRCLE('',#8867,0.399999999999991);
#1789=CIRCLE('',#8869,0.4);
#1790=CIRCLE('',#8870,0.4);
#1791=CIRCLE('',#8872,0.399999999999999);
#1792=CIRCLE('',#8873,0.4);
#1793=CIRCLE('',#8876,9.);
#1794=CIRCLE('',#8877,8.6);
#1795=CIRCLE('',#8880,9.);
#1796=CIRCLE('',#8881,9.);
#1797=CIRCLE('',#8883,4.);
#1798=CIRCLE('',#8887,0.4);
#1799=CIRCLE('',#8888,8.6);
#1800=CIRCLE('',#8890,7.4);
#1801=CIRCLE('',#8892,7.);
#1802=CIRCLE('',#8893,0.4);
#1803=CIRCLE('',#8895,7.);
#1804=CIRCLE('',#8896,7.);
#1805=CIRCLE('',#8898,6.6);
#1806=CIRCLE('',#8899,0.4);
#1807=CIRCLE('',#8901,6.);
#1808=CIRCLE('',#8903,5.);
#1809=CIRCLE('',#8905,5.);
#1810=CIRCLE('',#8910,8.866);
#1811=CIRCLE('',#8917,7.4455);
#1812=CIRCLE('',#8923,7.4455);
#1813=CIRCLE('',#8925,11.);
#1814=CIRCLE('',#8926,8.866);
#1815=CIRCLE('',#8928,11.);
#1816=CIRCLE('',#8930,7.);
#1817=CIRCLE('',#8932,7.);
#1818=CIRCLE('',#8938,0.399999999999998);
#1819=CIRCLE('',#8941,0.4);
#1820=CIRCLE('',#8944,0.399999999999997);
#1821=CIRCLE('',#8947,0.4);
#1822=CIRCLE('',#8954,0.399999999999997);
#1823=CIRCLE('',#8957,0.4);
#1824=CIRCLE('',#8959,1.3);
#1825=CIRCLE('',#8960,1.3);
#1826=CIRCLE('',#8961,1.3);
#1827=CIRCLE('',#8962,1.3);
#1828=CIRCLE('',#8965,2.);
#1829=CIRCLE('',#8966,2.);
#1830=CIRCLE('',#8969,2.);
#1831=CIRCLE('',#8970,2.);
#1832=CIRCLE('',#8972,2.);
#1833=CIRCLE('',#8973,2.);
#1834=CIRCLE('',#8976,2.);
#1835=CIRCLE('',#8977,2.);
#1836=CIRCLE('',#8980,1.3);
#1837=CIRCLE('',#8981,1.3);
#1838=CIRCLE('',#8982,1.3);
#1839=CIRCLE('',#8983,1.3);
#1840=CIRCLE('',#8985,0.4);
#1841=CIRCLE('',#8986,0.399999999999998);
#1842=CIRCLE('',#8998,0.496);
#1843=CIRCLE('',#9001,6.32479565138939);
#1844=CIRCLE('',#9003,5.93049029404341);
#1845=CIRCLE('',#9006,6.32479565138933);
#1846=CIRCLE('',#9008,0.496);
#1847=CIRCLE('',#9011,6.32479565138941);
#1848=CIRCLE('',#9013,5.93049029404341);
#1849=CIRCLE('',#9016,6.32479565138941);
#1850=CIRCLE('',#9019,0.496);
#1851=CIRCLE('',#9022,6.32479565138943);
#1852=CIRCLE('',#9024,0.496);
#1853=CIRCLE('',#9027,6.32479565138944);
#1854=CIRCLE('',#9029,6.32479565138933);
#1855=CIRCLE('',#9031,5.93049029404347);
#1856=CIRCLE('',#9032,5.93049029404347);
#1857=CIRCLE('',#9034,6.32479565138944);
#1858=CIRCLE('',#9036,5.93049029404341);
#1859=CIRCLE('',#9039,0.939230484541328);
#1860=CIRCLE('',#9040,0.1);
#1861=CIRCLE('',#9041,0.839230484541328);
#1862=CIRCLE('',#9043,2.15);
#1863=CIRCLE('',#9045,0.839230484541328);
#1864=CIRCLE('',#9047,0.96675);
#1865=CIRCLE('',#9049,0.96675);
#1866=CIRCLE('',#9052,6.32965591734106);
#1867=CIRCLE('',#9053,2.07563463599418);
#1868=CIRCLE('',#9054,2.07563463599418);
#1869=CIRCLE('',#9059,0.496);
#1870=CIRCLE('',#9062,6.32479565138939);
#1871=CIRCLE('',#9064,5.93049029404341);
#1872=CIRCLE('',#9067,6.32479565138933);
#1873=CIRCLE('',#9069,0.496);
#1874=CIRCLE('',#9072,6.32479565138941);
#1875=CIRCLE('',#9074,5.93049029404341);
#1876=CIRCLE('',#9077,6.32479565138941);
#1877=CIRCLE('',#9080,0.496);
#1878=CIRCLE('',#9083,6.32479565138943);
#1879=CIRCLE('',#9085,0.496);
#1880=CIRCLE('',#9088,6.32479565138944);
#1881=CIRCLE('',#9090,6.32479565138933);
#1882=CIRCLE('',#9092,5.93049029404347);
#1883=CIRCLE('',#9093,5.93049029404347);
#1884=CIRCLE('',#9095,6.32479565138944);
#1885=CIRCLE('',#9097,5.93049029404341);
#1886=CIRCLE('',#9100,0.939230484541328);
#1887=CIRCLE('',#9101,0.1);
#1888=CIRCLE('',#9102,0.839230484541328);
#1889=CIRCLE('',#9104,2.15);
#1890=CIRCLE('',#9106,0.839230484541328);
#1891=CIRCLE('',#9108,0.96675);
#1892=CIRCLE('',#9110,0.96675);
#1893=CIRCLE('',#9113,6.32965591734106);
#1894=CIRCLE('',#9114,2.07563463599418);
#1895=CIRCLE('',#9115,2.07563463599418);
#1896=CIRCLE('',#9120,0.496);
#1897=CIRCLE('',#9123,6.32479565138939);
#1898=CIRCLE('',#9125,5.93049029404341);
#1899=CIRCLE('',#9128,6.32479565138933);
#1900=CIRCLE('',#9130,0.496);
#1901=CIRCLE('',#9133,6.32479565138941);
#1902=CIRCLE('',#9135,5.93049029404341);
#1903=CIRCLE('',#9138,6.32479565138941);
#1904=CIRCLE('',#9141,0.496);
#1905=CIRCLE('',#9144,6.32479565138943);
#1906=CIRCLE('',#9146,0.496);
#1907=CIRCLE('',#9149,6.32479565138944);
#1908=CIRCLE('',#9151,6.32479565138933);
#1909=CIRCLE('',#9153,5.93049029404347);
#1910=CIRCLE('',#9154,5.93049029404347);
#1911=CIRCLE('',#9156,6.32479565138944);
#1912=CIRCLE('',#9158,5.93049029404341);
#1913=CIRCLE('',#9161,0.939230484541328);
#1914=CIRCLE('',#9162,0.1);
#1915=CIRCLE('',#9163,0.839230484541328);
#1916=CIRCLE('',#9165,2.15);
#1917=CIRCLE('',#9167,0.839230484541328);
#1918=CIRCLE('',#9169,0.96675);
#1919=CIRCLE('',#9171,0.96675);
#1920=CIRCLE('',#9174,6.32965591734106);
#1921=CIRCLE('',#9175,2.07563463599418);
#1922=CIRCLE('',#9176,2.07563463599418);
#1923=CIRCLE('',#9181,0.496);
#1924=CIRCLE('',#9184,6.32479565138939);
#1925=CIRCLE('',#9186,5.93049029404341);
#1926=CIRCLE('',#9189,6.32479565138933);
#1927=CIRCLE('',#9191,0.496);
#1928=CIRCLE('',#9194,6.32479565138941);
#1929=CIRCLE('',#9196,5.93049029404341);
#1930=CIRCLE('',#9199,6.32479565138941);
#1931=CIRCLE('',#9202,0.496);
#1932=CIRCLE('',#9205,6.32479565138943);
#1933=CIRCLE('',#9207,0.496);
#1934=CIRCLE('',#9210,6.32479565138944);
#1935=CIRCLE('',#9212,6.32479565138933);
#1936=CIRCLE('',#9214,5.93049029404347);
#1937=CIRCLE('',#9215,5.93049029404347);
#1938=CIRCLE('',#9217,6.32479565138944);
#1939=CIRCLE('',#9219,5.93049029404341);
#1940=CIRCLE('',#9222,0.939230484541328);
#1941=CIRCLE('',#9223,0.1);
#1942=CIRCLE('',#9224,0.839230484541328);
#1943=CIRCLE('',#9226,2.15);
#1944=CIRCLE('',#9228,0.839230484541328);
#1945=CIRCLE('',#9230,0.96675);
#1946=CIRCLE('',#9232,0.96675);
#1947=CIRCLE('',#9235,6.32965591734106);
#1948=CIRCLE('',#9236,2.07563463599418);
#1949=CIRCLE('',#9237,2.07563463599418);
#1950=B_SPLINE_CURVE_WITH_KNOTS('',3,(#11818,#11819,#11820,#11821,#11822,
#11823,#11824,#11825,#11826,#11827,#11828,#11829),.UNSPECIFIED.,.F.,.F.,
(4,2,2,2,2,4),(0.684266710157815,0.698356622095572,0.712446534033328,0.731803474638004,
0.751160415242679,0.78032220184246),.UNSPECIFIED.);
#1951=B_SPLINE_CURVE_WITH_KNOTS('',3,(#12568,#12569,#12570,#12571,#12572,
#12573,#12574,#12575,#12576,#12577,#12578,#12579,#12580,#12581),
 .UNSPECIFIED.,.F.,.F.,(4,2,2,2,2,2,4),(0.243709125451541,0.275010306594212,
0.329604611857381,0.356901764488965,0.38419891712055,0.398357188505934,
0.412515459891318),.UNSPECIFIED.);
#1952=B_SPLINE_CURVE_WITH_KNOTS('',3,(#13070,#13071,#13072,#13073,#13074),
 .UNSPECIFIED.,.F.,.F.,(4,1,4),(-0.0415580445559579,-0.020779022277979,
0.),.UNSPECIFIED.);
#1953=B_SPLINE_CURVE_WITH_KNOTS('',3,(#13075,#13076,#13077,#13078,#13079),
 .UNSPECIFIED.,.F.,.F.,(4,1,4),(0.,0.020779022277979,0.0415580445559579),
 .UNSPECIFIED.);
#1954=B_SPLINE_CURVE_WITH_KNOTS('',3,(#13165,#13166,#13167,#13168,#13169),
 .UNSPECIFIED.,.F.,.F.,(4,1,4),(-0.0415610054555056,-0.0207805027277528,
0.),.UNSPECIFIED.);
#1955=B_SPLINE_CURVE_WITH_KNOTS('',3,(#13170,#13171,#13172,#13173,#13174),
 .UNSPECIFIED.,.F.,.F.,(4,1,4),(0.,0.0207805027277528,0.0415610054555056),
 .UNSPECIFIED.);
#1956=B_SPLINE_CURVE_WITH_KNOTS('',3,(#13274,#13275,#13276,#13277,#13278),
 .UNSPECIFIED.,.F.,.F.,(4,1,4),(-0.0415580445559579,-0.0207790222779789,
0.),.UNSPECIFIED.);
#1957=B_SPLINE_CURVE_WITH_KNOTS('',3,(#13279,#13280,#13281,#13282,#13283),
 .UNSPECIFIED.,.F.,.F.,(4,1,4),(0.,0.0207790222779789,0.0415580445559579),
 .UNSPECIFIED.);
#1958=B_SPLINE_CURVE_WITH_KNOTS('',3,(#13369,#13370,#13371,#13372,#13373),
 .UNSPECIFIED.,.F.,.F.,(4,1,4),(-0.0415610054555052,-0.0207805027277526,
0.),.UNSPECIFIED.);
#1959=B_SPLINE_CURVE_WITH_KNOTS('',3,(#13374,#13375,#13376,#13377,#13378),
 .UNSPECIFIED.,.F.,.F.,(4,1,4),(0.,0.0207805027277526,0.0415610054555052),
 .UNSPECIFIED.);
#1960=B_SPLINE_CURVE_WITH_KNOTS('',3,(#13730,#13731,#13732,#13733,#13734,
#13735),.UNSPECIFIED.,.F.,.F.,(4,1,1,4),(0.,0.0435664957825988,0.0599039317010734,
0.0762413676195479),.UNSPECIFIED.);
#1961=B_SPLINE_CURVE_WITH_KNOTS('',3,(#13739,#13740,#13741,#13742,#13743,
#13744),.UNSPECIFIED.,.F.,.F.,(4,1,1,4),(-0.0762413676195479,-0.0599039317010734,
-0.0435664957825988,0.),.UNSPECIFIED.);
#1962=B_SPLINE_CURVE_WITH_KNOTS('',3,(#13778,#13779,#13780,#13781,#13782,
#13783),.UNSPECIFIED.,.F.,.F.,(4,1,1,4),(-0.0762406847351813,-0.0326745791722206,
-0.0163372895861103,0.),.UNSPECIFIED.);
#1963=B_SPLINE_CURVE_WITH_KNOTS('',3,(#13787,#13788,#13789,#13790,#13791,
#13792),.UNSPECIFIED.,.F.,.F.,(4,1,1,4),(0.,0.0163372895861103,0.0326745791722206,
0.0762406847351813),.UNSPECIFIED.);
#1964=B_SPLINE_CURVE_WITH_KNOTS('',3,(#13833,#13834,#13835,#13836,#13837,
#13838),.UNSPECIFIED.,.F.,.F.,(4,1,1,4),(-0.214017121799351,-0.0917216236282934,
-0.061147749085529,-3.96177645312185E-16),.UNSPECIFIED.);
#1965=B_SPLINE_CURVE_WITH_KNOTS('',3,(#13839,#13840,#13841,#13842,#13843,
#13844),.UNSPECIFIED.,.F.,.F.,(4,1,1,4),(3.96177645312185E-16,0.061147749085529,
0.0917216236282934,0.214017121799351),.UNSPECIFIED.);
#1966=B_SPLINE_CURVE_WITH_KNOTS('',3,(#13884,#13885,#13886,#13887,#13888,
#13889),.UNSPECIFIED.,.F.,.F.,(4,1,1,4),(-0.214026834508028,-0.152876310362877,
-0.0917257862177262,-2.01858731750029E-18),.UNSPECIFIED.);
#1967=B_SPLINE_CURVE_WITH_KNOTS('',3,(#13890,#13891,#13892,#13893,#13894,
#13895),.UNSPECIFIED.,.F.,.F.,(4,1,1,4),(2.01858731750029E-18,0.0917257862177262,
0.152876310362877,0.214026834508028),.UNSPECIFIED.);
#1968=B_SPLINE_CURVE_WITH_KNOTS('',3,(#13916,#13917,#13918,#13919,#13920,
#13921),.UNSPECIFIED.,.F.,.F.,(4,1,1,4),(-0.214017120895945,-0.0917216232411232,
-0.0611477488274177,-6.74145042959343E-15),.UNSPECIFIED.);
#1969=B_SPLINE_CURVE_WITH_KNOTS('',3,(#13958,#13959,#13960,#13961,#13962,
#13963),.UNSPECIFIED.,.F.,.F.,(4,1,1,4),(-0.0762406850317755,-0.0326745792993324,
-0.0163372896496662,0.),.UNSPECIFIED.);
#1970=B_SPLINE_CURVE_WITH_KNOTS('',3,(#13967,#13968,#13969,#13970,#13971,
#13972),.UNSPECIFIED.,.F.,.F.,(4,1,1,4),(0.,0.0163372896496662,0.0326745792993324,
0.0762406850317755),.UNSPECIFIED.);
#1971=B_SPLINE_CURVE_WITH_KNOTS('',3,(#14006,#14007,#14008,#14009,#14010,
#14011),.UNSPECIFIED.,.F.,.F.,(4,1,1,4),(7.01665201425609E-18,0.0435664948259872,
0.0599039303857324,0.0762413659454776),.UNSPECIFIED.);
#1972=B_SPLINE_CURVE_WITH_KNOTS('',3,(#14015,#14016,#14017,#14018,#14019,
#14020),.UNSPECIFIED.,.F.,.F.,(4,1,1,4),(-0.0762413659454776,-0.0599039303857324,
-0.0435664948259872,-7.01665201425609E-18),.UNSPECIFIED.);
#1973=B_SPLINE_CURVE_WITH_KNOTS('',3,(#14059,#14060,#14061,#14062,#14063,
#14064),.UNSPECIFIED.,.F.,.F.,(4,1,1,4),(6.74145042959343E-15,0.0611477488274177,
0.0917216232411232,0.214017120895945),.UNSPECIFIED.);
#1974=B_SPLINE_CURVE_WITH_KNOTS('',3,(#14102,#14103,#14104,#14105,#14106,
#14107),.UNSPECIFIED.,.F.,.F.,(4,1,1,4),(-0.214026834508028,-0.152876310362877,
-0.0917257862177262,0.),.UNSPECIFIED.);
#1975=B_SPLINE_CURVE_WITH_KNOTS('',3,(#14108,#14109,#14110,#14111,#14112,
#14113),.UNSPECIFIED.,.F.,.F.,(4,1,1,4),(0.,0.0917257862177262,0.152876310362877,
0.214026834508028),.UNSPECIFIED.);
#1976=B_SPLINE_CURVE_WITH_KNOTS('',3,(#14174,#14175,#14176,#14177,#14178,
#14179,#14180,#14181,#14182,#14183,#14184,#14185,#14186,#14187,#14188,#14189),
 .UNSPECIFIED.,.F.,.F.,(4,3,3,3,3,4),(-4.09289414414334,-3.92074098081279,
-3.43064835821119,-2.94055573560959,-2.45046311300799,-2.06120159751572),
 .UNSPECIFIED.);
#1977=B_SPLINE_CURVE_WITH_KNOTS('',3,(#14192,#14193,#14194,#14195,#14196,
#14197,#14198,#14199,#14200,#14201),.UNSPECIFIED.,.F.,.F.,(4,3,3,4),(0.,
0.490092622601601,0.980185245203199,1.10990010696217),.UNSPECIFIED.);
#1978=B_SPLINE_CURVE_WITH_KNOTS('',3,(#14206,#14207,#14208,#14209,#14210,
#14211,#14212,#14213,#14214,#14215,#14216,#14217,#14218,#14219,#14220,#14221,
#14222,#14223,#14224,#14225,#14226,#14227,#14228,#14229,#14230,#14231,#14232,
#14233,#14234,#14235,#14236,#14237,#14238,#14239,#14240,#14241,#14242,#14243,
#14244,#14245,#14246,#14247,#14248),.UNSPECIFIED.,.F.,.F.,(4,3,3,3,3,3,
3,3,3,3,3,3,3,3,4),(-10.3760794513229,-10.2919450746336,-9.80185245203197,
-9.31175982943038,-8.82166720682877,-8.33157458422717,-7.84148196162558,
-7.35138933902398,-6.86129671642238,-6.37120409382078,-5.88111147121918,
-5.39101884861759,-4.90092622601599,-4.41083360341439,-4.09289414414334),
 .UNSPECIFIED.);
#1979=B_SPLINE_CURVE_WITH_KNOTS('',3,(#14249,#14250,#14251,#14252,#14253,
#14254,#14255,#14256,#14257,#14258,#14259,#14260,#14261,#14262,#14263,#14264,
#14265,#14266,#14267,#14268,#14269,#14270,#14271,#14272,#14273,#14274,#14275,
#14276,#14277,#14278,#14279,#14280,#14281,#14282,#14283,#14284,#14285,#14286,
#14287,#14288,#14289,#14290,#14291),.UNSPECIFIED.,.F.,.F.,(4,3,3,3,3,3,
3,3,3,3,3,3,3,3,4),(1.10990010696217,1.4702778678048,1.9603704904064,2.450463113008,
2.94055573560959,3.43064835821119,3.92074098081279,4.41083360341439,4.90092622601598,
5.39101884861758,5.88111147121918,6.37120409382078,6.86129671642238,7.35138933902397,
7.39308541414175),.UNSPECIFIED.);
#1980=B_SPLINE_CURVE_WITH_KNOTS('',3,(#14296,#14297,#14298,#14299,#14300,
#14301,#14302,#14303,#14304,#14305,#14306,#14307,#14308,#14309,#14310,#14311,
#14312,#14313,#14314,#14315,#14316,#14317,#14318,#14319,#14320,#14321,#14322,
#14323,#14324,#14325,#14326,#14327,#14328,#14329,#14330,#14331,#14332,#14333,
#14334,#14335),.UNSPECIFIED.,.F.,.F.,(4,3,3,3,3,3,3,3,3,3,3,3,3,4),(-16.6592647585025,
-16.1730565458528,-15.6829639232512,-15.1928713006496,-14.702778678048,
-14.2126860554464,-13.7225934328448,-13.2325008102432,-12.7424081876416,
-12.25231556504,-11.7622229424384,-11.2721303198368,-10.7820376972352,-10.3760794513229),
 .UNSPECIFIED.);
#1981=B_SPLINE_CURVE_WITH_KNOTS('',3,(#14336,#14337,#14338,#14339,#14340,
#14341,#14342,#14343,#14344,#14345,#14346,#14347,#14348,#14349,#14350,#14351,
#14352,#14353,#14354,#14355,#14356,#14357,#14358,#14359,#14360,#14361,#14362,
#14363,#14364,#14365,#14366,#14367,#14368,#14369,#14370,#14371,#14372,#14373,
#14374,#14375),.UNSPECIFIED.,.F.,.F.,(4,3,3,3,3,3,3,3,3,3,3,3,3,4),(7.39308541414175,
7.84148196162557,8.33157458422717,8.82166720682877,9.31175982943037,9.80185245203197,
10.2919450746336,10.7820376972352,11.2721303198368,11.7622229424384,12.25231556504,
12.7424081876416,13.2325008102432,13.6762707213213),.UNSPECIFIED.);
#1982=B_SPLINE_CURVE_WITH_KNOTS('',3,(#14380,#14381,#14382,#14383,#14384,
#14385,#14386,#14387,#14388,#14389,#14390,#14391,#14392,#14393,#14394,#14395,
#14396,#14397,#14398,#14399,#14400,#14401,#14402,#14403,#14404,#14405,#14406,
#14407,#14408,#14409,#14410,#14411,#14412,#14413,#14414,#14415,#14416,#14417,
#14418,#14419,#14420,#14421,#14422),.UNSPECIFIED.,.F.,.F.,(4,3,3,3,3,3,
3,3,3,3,3,3,3,3,4),(-22.9424500656821,-22.5442606396735,-22.0541680170719,
-21.5640753944703,-21.0739827718687,-20.5838901492671,-20.0937975266655,
-19.6037049040639,-19.1136122814623,-18.6235196588607,-18.1334270362591,
-17.6433344136575,-17.153241791056,-16.6631491684543,-16.6592647585025),
 .UNSPECIFIED.);
#1983=B_SPLINE_CURVE_WITH_KNOTS('',3,(#14423,#14424,#14425,#14426,#14427,
#14428,#14429,#14430,#14431,#14432,#14433,#14434,#14435,#14436,#14437,#14438,
#14439,#14440,#14441,#14442,#14443,#14444,#14445,#14446,#14447,#14448,#14449,
#14450,#14451,#14452,#14453,#14454,#14455,#14456,#14457,#14458,#14459,#14460,
#14461,#14462,#14463,#14464,#14465),.UNSPECIFIED.,.F.,.F.,(4,3,3,3,3,3,
3,3,3,3,3,3,3,3,4),(13.6762707213213,13.7225934328448,14.2126860554464,
14.702778678048,15.1928713006496,15.6829639232512,16.1730565458528,16.6631491684543,
17.1532417910559,17.6433344136575,18.1334270362591,18.6235196588607,19.1136122814623,
19.6037049040639,19.9594560285009),.UNSPECIFIED.);
#1984=B_SPLINE_CURVE_WITH_KNOTS('',3,(#14470,#14471,#14472,#14473,#14474,
#14475,#14476,#14477,#14478,#14479,#14480,#14481,#14482,#14483,#14484,#14485,
#14486,#14487,#14488,#14489,#14490,#14491,#14492,#14493,#14494,#14495,#14496,
#14497,#14498,#14499,#14500,#14501,#14502,#14503,#14504,#14505,#14506,#14507,
#14508,#14509,#14510,#14511,#14512),.UNSPECIFIED.,.F.,.F.,(4,3,3,3,3,3,
3,3,3,3,3,3,3,3,4),(-29.2256353728617,-28.9154647334943,-28.4253721108927,
-27.9352794882911,-27.4451868656895,-26.9550942430879,-26.4650016204863,
-25.9749089978847,-25.4848163752831,-24.9947237526815,-24.5046311300799,
-24.0145385074783,-23.5244458848767,-23.0343532622751,-22.9424500656821),
 .UNSPECIFIED.);
#1985=B_SPLINE_CURVE_WITH_KNOTS('',3,(#14513,#14514,#14515,#14516,#14517,
#14518,#14519,#14520,#14521,#14522,#14523,#14524,#14525,#14526,#14527,#14528,
#14529,#14530,#14531,#14532,#14533,#14534,#14535,#14536,#14537,#14538,#14539,
#14540,#14541,#14542,#14543,#14544,#14545,#14546,#14547,#14548,#14549,#14550,
#14551,#14552,#14553,#14554,#14555),.UNSPECIFIED.,.F.,.F.,(4,3,3,3,3,3,
3,3,3,3,3,3,3,3,4),(19.9594560285009,20.0937975266655,20.5838901492671,
21.0739827718687,21.5640753944703,22.0541680170719,22.5442606396735,23.0343532622751,
23.5244458848767,24.0145385074783,24.5046311300799,24.9947237526815,25.4848163752831,
25.9749089978847,26.2426413356805),.UNSPECIFIED.);
#1986=B_SPLINE_CURVE_WITH_KNOTS('',3,(#14560,#14561,#14562,#14563,#14564,
#14565,#14566,#14567,#14568,#14569,#14570,#14571,#14572,#14573,#14574,#14575,
#14576,#14577,#14578,#14579,#14580,#14581,#14582,#14583,#14584,#14585,#14586,
#14587,#14588,#14589,#14590,#14591,#14592,#14593,#14594,#14595,#14596,#14597,
#14598,#14599,#14600,#14601,#14602),.UNSPECIFIED.,.F.,.F.,(4,3,3,3,3,3,
3,3,3,3,3,3,3,3,4),(-35.5088206800413,-35.2866688273151,-34.7965762047135,
-34.3064835821119,-33.8163909595103,-33.3262983369087,-32.8362057143071,
-32.3461130917055,-31.8560204691039,-31.3659278465023,-30.8758352239007,
-30.3857426012991,-29.8956499786975,-29.4055573560959,-29.2256353728617),
 .UNSPECIFIED.);
#1987=B_SPLINE_CURVE_WITH_KNOTS('',3,(#14603,#14604,#14605,#14606,#14607,
#14608,#14609,#14610,#14611,#14612,#14613,#14614,#14615,#14616,#14617,#14618,
#14619,#14620,#14621,#14622,#14623,#14624,#14625,#14626,#14627,#14628,#14629,
#14630,#14631,#14632,#14633,#14634,#14635,#14636,#14637,#14638,#14639,#14640,
#14641,#14642,#14643,#14644,#14645),.UNSPECIFIED.,.F.,.F.,(4,3,3,3,3,3,
3,3,3,3,3,3,3,3,4),(26.2426413356805,26.4650016204863,26.9550942430879,
27.4451868656895,27.9352794882911,28.4253721108927,28.9154647334943,29.4055573560959,
29.8956499786975,30.3857426012991,30.8758352239007,31.3659278465023,31.8560204691039,
32.3461130917055,32.5258266428601),.UNSPECIFIED.);
#1988=B_SPLINE_CURVE_WITH_KNOTS('',3,(#14651,#14652,#14653,#14654,#14655,
#14656,#14657,#14658,#14659,#14660,#14661,#14662,#14663,#14664,#14665,#14666),
 .UNSPECIFIED.,.F.,.F.,(4,1,1,1,1,1,1,1,1,1,1,1,1,4),(40.8407044966673,
41.0206264799015,41.5107191025031,42.0008117251047,42.4909043477063,42.9809969703079,
43.4710895929095,43.9611822155111,44.4512748381127,44.9413674607143,45.4314600833159,
45.9215527059175,46.4116453285191,46.8009068440113),.UNSPECIFIED.);
#1989=B_SPLINE_CURVE_WITH_KNOTS('',3,(#14669,#14670,#14671,#14672,#14673,
#14674,#14675,#14676,#14677,#14678,#14679,#14680,#14681),.UNSPECIFIED.,
 .F.,.F.,(4,1,1,1,1,1,1,1,1,1,4),(40.8407044966673,41.1510835681143,41.6411761907159,
42.1312688133175,42.6213614359191,43.1114540585207,43.6015466811223,44.0916393037239,
44.5817319263255,45.0718245489271,45.5619171715287),.UNSPECIFIED.);
#1990=B_SPLINE_CURVE_WITH_KNOTS('',3,(#14686,#14687,#14688,#14689,#14690,
#14691,#14692,#14693,#14694,#14695,#14696,#14697,#14698,#14699,#14700,#14701,
#14702),.UNSPECIFIED.,.F.,.F.,(4,1,1,1,1,1,1,1,1,1,1,1,1,1,4),(34.5575191894877,
34.6494223860807,35.1395150086823,35.6296076312839,36.1197002538855,36.6097928764871,
37.0998854990887,37.5899781216903,38.0800707442919,38.5701633668935,39.0602559894951,
39.5503486120967,40.0404412346983,40.5305338572999,40.8407044966673),
 .UNSPECIFIED.);
#1991=B_SPLINE_CURVE_WITH_KNOTS('',3,(#14703,#14704,#14705,#14706,#14707,
#14708,#14709,#14710,#14711,#14712,#14713,#14714,#14715,#14716,#14717,#14718,
#14719),.UNSPECIFIED.,.F.,.F.,(4,1,1,1,1,1,1,1,1,1,1,1,1,1,4),(34.5575191894877,
34.7798794742935,35.2699720968951,35.7600647194967,36.2501573420983,36.7402499646999,
37.2303425873015,37.7204352099031,38.2105278325047,38.7006204551063,39.1907130777079,
39.6808057003095,40.1708983229111,40.6609909455127,40.8407044966673),
 .UNSPECIFIED.);
#1992=B_SPLINE_CURVE_WITH_KNOTS('',3,(#14724,#14725,#14726,#14727,#14728,
#14729,#14730,#14731,#14732,#14733,#14734,#14735,#14736,#14737,#14738,#14739,
#14740),.UNSPECIFIED.,.F.,.F.,(4,1,1,1,1,1,1,1,1,1,1,1,1,1,4),(28.2743338823081,
28.2782182922599,28.7683109148615,29.2584035374631,29.7484961600647,30.2385887826663,
30.7286814052679,31.2187740278695,31.7088666504711,32.1989592730727,32.6890518956743,
33.1791445182759,33.6692371408775,34.1593297634791,34.5575191894877),
 .UNSPECIFIED.);
#1993=B_SPLINE_CURVE_WITH_KNOTS('',3,(#14741,#14742,#14743,#14744,#14745,
#14746,#14747,#14748,#14749,#14750,#14751,#14752,#14753,#14754,#14755,#14756,
#14757),.UNSPECIFIED.,.F.,.F.,(4,1,1,1,1,1,1,1,1,1,1,1,1,1,4),(28.2743338823081,
28.4086753804727,28.8987680030743,29.3888606256759,29.8789532482775,30.3690458708791,
30.8591384934807,31.3492311160823,31.8393237386839,32.3294163612855,32.8195089838871,
33.3096016064887,33.7996942290903,34.2897868516919,34.5575191894877),
 .UNSPECIFIED.);
#1994=B_SPLINE_CURVE_WITH_KNOTS('',3,(#14762,#14763,#14764,#14765,#14766,
#14767,#14768,#14769,#14770,#14771,#14772,#14773,#14774,#14775,#14776,#14777),
 .UNSPECIFIED.,.F.,.F.,(4,1,1,1,1,1,1,1,1,1,1,1,1,4),(21.9911485751285,
22.3971068210408,22.8871994436423,23.3772920662439,23.8673846888455,24.3574773114471,
24.8475699340487,25.3376625566503,25.8277551792519,26.3178478018535,26.8079404244551,
27.2980330470567,27.7881256696583,28.2743338823081),.UNSPECIFIED.);
#1995=B_SPLINE_CURVE_WITH_KNOTS('',3,(#14778,#14779,#14780,#14781,#14782,
#14783,#14784,#14785,#14786,#14787,#14788,#14789,#14790,#14791,#14792,#14793,
#14794),.UNSPECIFIED.,.F.,.F.,(4,1,1,1,1,1,1,1,1,1,1,1,1,1,4),(21.9911485751286,
22.0374712866519,22.5275639092535,23.0176565318551,23.5077491544567,23.9978417770583,
24.4879343996599,24.9780270222615,25.4681196448631,25.9582122674647,26.4483048900663,
26.9383975126679,27.4284901352695,27.9185827578711,28.2743338823081),
 .UNSPECIFIED.);
#1996=B_SPLINE_CURVE_WITH_KNOTS('',3,(#14799,#14800,#14801,#14802,#14803,
#14804,#14805,#14806,#14807,#14808,#14809,#14810,#14811,#14812,#14813,#14814,
#14815),.UNSPECIFIED.,.F.,.F.,(4,1,1,1,1,1,1,1,1,1,1,1,1,1,4),(15.707963267949,
16.02590272722,16.5159953498216,17.0060879724232,17.4961805950248,17.9862732176264,
18.476365840228,18.9664584628296,19.4565510854312,19.9466437080328,20.4367363306344,
20.926828953236,21.4169215758376,21.9070141984391,21.9911485751285),
 .UNSPECIFIED.);
#1997=B_SPLINE_CURVE_WITH_KNOTS('',3,(#14816,#14817,#14818,#14819,#14820,
#14821,#14822,#14823,#14824,#14825,#14826,#14827,#14828,#14829,#14830,#14831),
 .UNSPECIFIED.,.F.,.F.,(4,1,1,1,1,1,1,1,1,1,1,1,1,4),(15.707963267949,16.1563598154328,
16.6464524380344,17.136545060636,17.6266376832376,18.1167303058392,18.6068229284408,
19.0969155510424,19.587008173644,20.0771007962456,20.5671934188472,21.0572860414487,
21.5473786640503,21.9911485751286),.UNSPECIFIED.);
#1998=B_SPLINE_CURVE_WITH_KNOTS('',3,(#15149,#15150,#15151,#15152,#15153,
#15154,#15155,#15156,#15157,#15158,#15159,#15160,#15161,#15162,#15163,#15164,
#15165,#15166,#15167,#15168,#15169,#15170,#15171,#15172,#15173,#15174,#15175,
#15176,#15177,#15178,#15179,#15180,#15181,#15182,#15183,#15184,#15185,#15186,
#15187,#15188,#15189,#15190,#15191,#15192,#15193,#15194,#15195,#15196,#15197,
#15198,#15199,#15200,#15201,#15202,#15203,#15204,#15205,#15206,#15207,#15208,
#15209,#15210,#15211,#15212,#15213,#15214,#15215,#15216,#15217,#15218,#15219,
#15220,#15221,#15222,#15223,#15224,#15225,#15226,#15227,#15228,#15229,#15230,
#15231,#15232,#15233,#15234,#15235,#15236,#15237,#15238,#15239,#15240,#15241,
#15242,#15243,#15244,#15245,#15246,#15247,#15248,#15249,#15250,#15251,#15252,
#15253,#15254,#15255,#15256,#15257,#15258,#15259,#15260,#15261,#15262,#15263,
#15264,#15265,#15266),.UNSPECIFIED.,.F.,.F.,(4,3,3,3,3,3,3,3,3,3,3,3,3,
3,3,3,3,3,3,3,3,3,3,3,3,3,3,3,3,3,3,3,3,3,3,3,3,3,3,4),(-0.844212290556747,
-0.810702516157805,-0.79964270029283,-0.765919058559404,-0.74366337577556,
-0.731523639816212,-0.726514248567387,-0.691854085497703,-0.658890756431271,
-0.626284026666266,-0.621345574606071,-0.617273921855323,-0.587873596288652,
-0.555368241117901,-0.522812249480479,-0.490470932706205,-0.463805273987372,
-0.457610503699064,-0.453861600002129,-0.422127751490738,-0.390594093312638,
-0.383808297830876,-0.35202939501847,-0.320473779186617,-0.303891190705963,
-0.300021989550331,-0.296270020852446,-0.265284115169516,-0.234382559785099,
-0.203906579402215,-0.187813071341382,-0.164336437423709,-0.154065410084727,
-0.148511188072182,-0.144961719969282,-0.114842428131466,-0.08467071113935,
-0.0547168723966001,-0.025375144198552,0.),.UNSPECIFIED.);
#1999=B_SPLINE_CURVE_WITH_KNOTS('',3,(#15267,#15268,#15269,#15270,#15271,
#15272,#15273,#15274,#15275,#15276,#15277,#15278,#15279,#15280,#15281,#15282,
#15283,#15284,#15285),.UNSPECIFIED.,.F.,.F.,(4,3,3,3,3,3,4),(32.5258266428601,
32.8362057143071,33.3262983369087,33.8163909595103,34.3064835821119,34.7965762047135,
35.1858377202057),.UNSPECIFIED.);
#2000=B_SPLINE_CURVE_WITH_KNOTS('',3,(#15287,#15288,#15289,#15290,#15291,
#15292,#15293,#15294,#15295,#15296,#15297,#15298,#15299,#15300,#15301,#15302,
#15303,#15304,#15305,#15306,#15307,#15308,#15309,#15310,#15311,#15312,#15313,
#15314,#15315,#15316,#15317,#15318,#15319,#15320,#15321,#15322,#15323,#15324,
#15325,#15326,#15327,#15328,#15329,#15330,#15331,#15332,#15333,#15334,#15335,
#15336,#15337,#15338,#15339,#15340,#15341,#15342,#15343,#15344,#15345,#15346,
#15347,#15348,#15349,#15350,#15351,#15352,#15353,#15354,#15355,#15356,#15357,
#15358,#15359,#15360,#15361,#15362,#15363,#15364,#15365,#15366,#15367,#15368,
#15369,#15370,#15371,#15372,#15373,#15374,#15375,#15376,#15377,#15378,#15379,
#15380,#15381,#15382,#15383,#15384,#15385,#15386,#15387,#15388,#15389,#15390,
#15391,#15392,#15393,#15394,#15395,#15396,#15397,#15398,#15399,#15400,#15401,
#15402,#15403,#15404),.UNSPECIFIED.,.F.,.F.,(4,3,3,3,3,3,3,3,3,3,3,3,3,
3,3,3,3,3,3,3,3,3,3,3,3,3,3,3,3,3,3,3,3,3,3,3,3,3,3,4),(0.,0.0300123333223647,
0.037944150695711,0.067648175262101,0.097699819048293,0.127901365024015,
0.14035318466012,0.145834882567896,0.149682014312836,0.180339090874683,
0.211336159587801,0.227515922112858,0.258328578058299,0.279183136595314,
0.297430875315202,0.302279216021489,0.33366950401744,0.365348220132565,
0.397119184767528,0.425165046354417,0.450865820177805,0.4562230243213,0.459845019664696,
0.491563428307749,0.52375659439166,0.556312891291814,0.588829688145416,
0.609800462543468,0.616688207028659,0.62066244680986,0.63077123694152,0.663389038839408,
0.696389124596628,0.714867020341643,0.72933984329808,0.734034406103895,
0.767602826667506,0.801324953467599,0.834922838602097,0.844212290556745),
 .UNSPECIFIED.);
#2001=B_SPLINE_CURVE_WITH_KNOTS('',3,(#15405,#15406,#15407,#15408,#15409,
#15410,#15411,#15412,#15413,#15414,#15415,#15416,#15417,#15418,#15419),
 .UNSPECIFIED.,.F.,.F.,(4,1,1,1,1,1,1,1,1,1,1,1,4),(10.3760794513229,10.7653409668152,
11.2554335894168,11.7455262120184,12.23561883462,12.7257114572216,13.2158040798232,
13.7058967024248,14.1959893250264,14.686081947628,15.1761745702296,15.6662671928312,
15.707963267949),.UNSPECIFIED.);
#2002=B_SPLINE_CURVE_WITH_KNOTS('',3,(#15423,#15424,#15425,#15426,#15427,
#15428,#15429,#15430,#15431,#15432,#15433,#15434),.UNSPECIFIED.,.F.,.F.,
(4,1,1,1,1,1,1,1,1,4),(11.6150691238056,12.1051617464072,12.5952543690088,
13.0853469916104,13.575439614212,14.0655322368136,14.5556248594152,15.0457174820168,
15.5358101046184,15.707963267949),.UNSPECIFIED.);
#2003=B_SPLINE_CURVE_WITH_KNOTS('',3,(#15752,#15753,#15754,#15755,#15756,
#15757,#15758,#15759,#15760,#15761,#15762,#15763,#15764,#15765,#15766,#15767,
#15768,#15769,#15770,#15771,#15772,#15773,#15774,#15775,#15776,#15777,#15778,
#15779,#15780,#15781,#15782,#15783,#15784,#15785,#15786,#15787,#15788,#15789,
#15790,#15791,#15792,#15793,#15794,#15795,#15796,#15797,#15798,#15799,#15800,
#15801,#15802,#15803,#15804,#15805,#15806,#15807,#15808,#15809,#15810,#15811,
#15812,#15813,#15814,#15815,#15816,#15817,#15818,#15819,#15820,#15821,#15822,
#15823,#15824,#15825,#15826,#15827,#15828,#15829,#15830,#15831,#15832,#15833,
#15834,#15835,#15836,#15837,#15838,#15839,#15840,#15841,#15842,#15843,#15844,
#15845,#15846,#15847,#15848,#15849,#15850,#15851,#15852,#15853,#15854,#15855,
#15856,#15857,#15858,#15859,#15860,#15861,#15862,#15863,#15864,#15865,#15866),
 .UNSPECIFIED.,.F.,.F.,(4,3,3,3,3,3,3,3,3,3,3,3,3,3,3,3,3,3,3,3,3,3,3,3,
3,3,3,3,3,3,3,3,3,3,3,3,3,3,4),(-0.847325527525887,-0.817174099062059,-0.809288442555136,
-0.779387793163181,-0.759391304785787,-0.749759381505324,-0.745433732408388,
-0.713929270842299,-0.683194914240082,-0.651305400192057,-0.64722148049575,
-0.619415886144032,-0.588655017110779,-0.557502684196823,-0.526148419840108,
-0.499868882928017,-0.495563318542414,-0.491909397242946,-0.460075674578441,
-0.427928427987543,-0.421030272191743,-0.389124013627929,-0.357018072660473,
-0.339205138860963,-0.335445901760091,-0.331555114265235,-0.298995857778172,
-0.266153422414382,-0.233231717588429,-0.214514602264393,-0.187700276981344,
-0.17596900967001,-0.170411920862904,-0.166565393534998,-0.133649950991215,
-0.100083272956281,-0.0663782103294436,-0.0328789002448827,0.),
 .UNSPECIFIED.);
#2004=B_SPLINE_CURVE_WITH_KNOTS('',3,(#15867,#15868,#15869,#15870,#15871,
#15872,#15873,#15874,#15875,#15876,#15877,#15878,#15879,#15880,#15881,#15882,
#15883,#15884,#15885,#15886,#15887,#15888,#15889,#15890,#15891,#15892,#15893,
#15894,#15895,#15896,#15897,#15898,#15899,#15900,#15901,#15902,#15903,#15904,
#15905,#15906,#15907,#15908,#15909,#15910,#15911,#15912,#15913,#15914,#15915,
#15916,#15917,#15918,#15919,#15920,#15921,#15922,#15923,#15924,#15925,#15926,
#15927,#15928,#15929,#15930,#15931,#15932,#15933,#15934,#15935,#15936,#15937,
#15938,#15939,#15940,#15941,#15942,#15943,#15944,#15945,#15946,#15947,#15948,
#15949,#15950,#15951,#15952,#15953,#15954,#15955,#15956,#15957,#15958,#15959,
#15960,#15961,#15962,#15963,#15964,#15965,#15966,#15967,#15968,#15969,#15970,
#15971,#15972,#15973,#15974,#15975,#15976,#15977,#15978,#15979,#15980,#15981,
#15982,#15983,#15984),.UNSPECIFIED.,.F.,.F.,(4,3,3,3,3,3,3,3,3,3,3,3,3,
3,3,3,3,3,3,3,3,3,3,3,3,3,3,3,3,3,3,3,3,3,3,3,3,3,3,4),(0.,0.0335918750467964,
0.0447567410947651,0.0784369868399077,0.112112469599625,0.145519061555296,
0.159542948288381,0.168194038831209,0.172781428939712,0.205672698986681,
0.238354352518147,0.257710155419976,0.290609738695869,0.323232443047843,
0.333001221767483,0.337747248940037,0.36989025535088,0.401969735275938,
0.433590777177308,0.462539571533553,0.487114992308667,0.492221114477958,
0.497620252043672,0.528870508315497,0.561438615670238,0.592551446157557,
0.623302493496337,0.641222715615399,0.647822694022932,0.652667114174829,
0.65914293773446,0.689868853330734,0.720585825371081,0.736428288140424,
0.748930866867351,0.752874528704484,0.783020499126383,0.812949359166843,
0.842371062577774,0.847325527525827),.UNSPECIFIED.);
#2005=B_SPLINE_CURVE_WITH_KNOTS('',3,(#15985,#15986,#15987,#15988,#15989,
#15990,#15991,#15992,#15993,#15994,#15995,#15996,#15997),.UNSPECIFIED.,
 .F.,.F.,(4,3,3,3,4),(-37.2470393177215,-36.7569466951199,-36.2668540725183,
-35.7767614499167,-35.5088206800413),.UNSPECIFIED.);
#2006=B_SPLINE_CURVE_WITH_KNOTS('',3,(#16263,#16264,#16265,#16266,#16267,
#16268,#16269,#16270,#16271,#16272,#16273,#16274,#16275,#16276,#16277),
 .UNSPECIFIED.,.F.,.F.,(4,2,2,3,2,2,4),(-0.0374758352523592,-0.0373394553501654,
-0.0186697276750827,0.,0.0186697276750831,0.0373394553501661,0.0374758352523223),
 .UNSPECIFIED.);
#2007=B_SPLINE_CURVE_WITH_KNOTS('',3,(#16305,#16306,#16307,#16308,#16309,
#16310,#16311,#16312,#16313,#16314,#16315,#16316,#16317,#16318,#16319),
 .UNSPECIFIED.,.F.,.F.,(4,2,2,3,2,2,4),(-0.0374758352523656,-0.0373394553501654,
-0.0186697276750827,0.,0.0186697276750831,0.0373394553501662,0.0374758352523289),
 .UNSPECIFIED.);
#2008=B_SPLINE_CURVE_WITH_KNOTS('',3,(#16344,#16345,#16346,#16347,#16348,
#16349,#16350,#16351,#16352,#16353,#16354,#16355,#16356,#16357,#16358),
 .UNSPECIFIED.,.F.,.F.,(4,2,2,3,2,2,4),(-0.0374758352524519,-0.0373394553501659,
-0.0186697276750829,0.,0.0186697276750829,0.0373394553501658,0.0374758352524142),
 .UNSPECIFIED.);
#2009=B_SPLINE_CURVE_WITH_KNOTS('',3,(#16374,#16375,#16376,#16377,#16378,
#16379,#16380,#16381,#16382,#16383,#16384,#16385,#16386,#16387,#16388),
 .UNSPECIFIED.,.F.,.F.,(4,2,2,3,2,2,4),(-0.0374758352524171,-0.0373394553501658,
-0.0186697276750829,0.,0.018669727675083,0.037339455350166,0.0374758352523797),
 .UNSPECIFIED.);
#2010=B_SPLINE_CURVE_WITH_KNOTS('',3,(#16449,#16450,#16451,#16452,#16453,
#16454,#16455,#16456,#16457,#16458,#16459,#16460,#16461,#16462,#16463),
 .UNSPECIFIED.,.F.,.F.,(4,2,2,3,2,2,4),(-0.0374758352523592,-0.0373394553501654,
-0.0186697276750827,0.,0.0186697276750831,0.0373394553501661,0.0374758352523223),
 .UNSPECIFIED.);
#2011=B_SPLINE_CURVE_WITH_KNOTS('',3,(#16491,#16492,#16493,#16494,#16495,
#16496,#16497,#16498,#16499,#16500,#16501,#16502,#16503,#16504,#16505),
 .UNSPECIFIED.,.F.,.F.,(4,2,2,3,2,2,4),(-0.0374758352523656,-0.0373394553501654,
-0.0186697276750827,0.,0.0186697276750831,0.0373394553501662,0.0374758352523289),
 .UNSPECIFIED.);
#2012=B_SPLINE_CURVE_WITH_KNOTS('',3,(#16530,#16531,#16532,#16533,#16534,
#16535,#16536,#16537,#16538,#16539,#16540,#16541,#16542,#16543,#16544),
 .UNSPECIFIED.,.F.,.F.,(4,2,2,3,2,2,4),(-0.0374758352524519,-0.0373394553501659,
-0.0186697276750829,0.,0.0186697276750829,0.0373394553501658,0.0374758352524142),
 .UNSPECIFIED.);
#2013=B_SPLINE_CURVE_WITH_KNOTS('',3,(#16560,#16561,#16562,#16563,#16564,
#16565,#16566,#16567,#16568,#16569,#16570,#16571,#16572,#16573,#16574),
 .UNSPECIFIED.,.F.,.F.,(4,2,2,3,2,2,4),(-0.0374758352524171,-0.0373394553501658,
-0.0186697276750829,0.,0.018669727675083,0.037339455350166,0.0374758352523797),
 .UNSPECIFIED.);
#2014=B_SPLINE_CURVE_WITH_KNOTS('',3,(#16635,#16636,#16637,#16638,#16639,
#16640,#16641,#16642,#16643,#16644,#16645,#16646,#16647,#16648,#16649),
 .UNSPECIFIED.,.F.,.F.,(4,2,2,3,2,2,4),(-0.0374758352523592,-0.0373394553501654,
-0.0186697276750827,0.,0.0186697276750831,0.0373394553501661,0.0374758352523223),
 .UNSPECIFIED.);
#2015=B_SPLINE_CURVE_WITH_KNOTS('',3,(#16677,#16678,#16679,#16680,#16681,
#16682,#16683,#16684,#16685,#16686,#16687,#16688,#16689,#16690,#16691),
 .UNSPECIFIED.,.F.,.F.,(4,2,2,3,2,2,4),(-0.0374758352523656,-0.0373394553501654,
-0.0186697276750827,0.,0.0186697276750831,0.0373394553501662,0.0374758352523289),
 .UNSPECIFIED.);
#2016=B_SPLINE_CURVE_WITH_KNOTS('',3,(#16716,#16717,#16718,#16719,#16720,
#16721,#16722,#16723,#16724,#16725,#16726,#16727,#16728,#16729,#16730),
 .UNSPECIFIED.,.F.,.F.,(4,2,2,3,2,2,4),(-0.0374758352524519,-0.0373394553501659,
-0.0186697276750829,0.,0.0186697276750829,0.0373394553501658,0.0374758352524142),
 .UNSPECIFIED.);
#2017=B_SPLINE_CURVE_WITH_KNOTS('',3,(#16746,#16747,#16748,#16749,#16750,
#16751,#16752,#16753,#16754,#16755,#16756,#16757,#16758,#16759,#16760),
 .UNSPECIFIED.,.F.,.F.,(4,2,2,3,2,2,4),(-0.0374758352524171,-0.0373394553501658,
-0.0186697276750829,0.,0.018669727675083,0.037339455350166,0.0374758352523797),
 .UNSPECIFIED.);
#2018=B_SPLINE_CURVE_WITH_KNOTS('',3,(#16821,#16822,#16823,#16824,#16825,
#16826,#16827,#16828,#16829,#16830,#16831,#16832,#16833,#16834,#16835),
 .UNSPECIFIED.,.F.,.F.,(4,2,2,3,2,2,4),(-0.0374758352523592,-0.0373394553501654,
-0.0186697276750827,0.,0.0186697276750831,0.0373394553501661,0.0374758352523223),
 .UNSPECIFIED.);
#2019=B_SPLINE_CURVE_WITH_KNOTS('',3,(#16863,#16864,#16865,#16866,#16867,
#16868,#16869,#16870,#16871,#16872,#16873,#16874,#16875,#16876,#16877),
 .UNSPECIFIED.,.F.,.F.,(4,2,2,3,2,2,4),(-0.0374758352523656,-0.0373394553501654,
-0.0186697276750827,0.,0.0186697276750831,0.0373394553501662,0.0374758352523289),
 .UNSPECIFIED.);
#2020=B_SPLINE_CURVE_WITH_KNOTS('',3,(#16902,#16903,#16904,#16905,#16906,
#16907,#16908,#16909,#16910,#16911,#16912,#16913,#16914,#16915,#16916),
 .UNSPECIFIED.,.F.,.F.,(4,2,2,3,2,2,4),(-0.0374758352524519,-0.0373394553501659,
-0.0186697276750829,0.,0.0186697276750829,0.0373394553501658,0.0374758352524142),
 .UNSPECIFIED.);
#2021=B_SPLINE_CURVE_WITH_KNOTS('',3,(#16932,#16933,#16934,#16935,#16936,
#16937,#16938,#16939,#16940,#16941,#16942,#16943,#16944,#16945,#16946),
 .UNSPECIFIED.,.F.,.F.,(4,2,2,3,2,2,4),(-0.0374758352524171,-0.0373394553501658,
-0.0186697276750829,0.,0.018669727675083,0.037339455350166,0.0374758352523797),
 .UNSPECIFIED.);
#2022=LINE('',#11816,#2600);
#2023=LINE('',#11833,#2601);
#2024=LINE('',#11837,#2602);
#2025=LINE('',#11841,#2603);
#2026=LINE('',#11843,#2604);
#2027=LINE('',#11844,#2605);
#2028=LINE('',#11848,#2606);
#2029=LINE('',#11850,#2607);
#2030=LINE('',#11851,#2608);
#2031=LINE('',#11853,#2609);
#2032=LINE('',#11854,#2610);
#2033=LINE('',#11858,#2611);
#2034=LINE('',#11861,#2612);
#2035=LINE('',#11863,#2613);
#2036=LINE('',#11864,#2614);
#2037=LINE('',#11869,#2615);
#2038=LINE('',#11874,#2616);
#2039=LINE('',#11875,#2617);
#2040=LINE('',#11876,#2618);
#2041=LINE('',#11879,#2619);
#2042=LINE('',#11881,#2620);
#2043=LINE('',#11882,#2621);
#2044=LINE('',#11885,#2622);
#2045=LINE('',#11887,#2623);
#2046=LINE('',#11889,#2624);
#2047=LINE('',#11891,#2625);
#2048=LINE('',#11892,#2626);
#2049=LINE('',#11895,#2627);
#2050=LINE('',#11899,#2628);
#2051=LINE('',#11903,#2629);
#2052=LINE('',#11905,#2630);
#2053=LINE('',#11907,#2631);
#2054=LINE('',#11909,#2632);
#2055=LINE('',#11915,#2633);
#2056=LINE('',#11924,#2634);
#2057=LINE('',#11927,#2635);
#2058=LINE('',#11931,#2636);
#2059=LINE('',#11935,#2637);
#2060=LINE('',#11939,#2638);
#2061=LINE('',#11942,#2639);
#2062=LINE('',#11947,#2640);
#2063=LINE('',#11950,#2641);
#2064=LINE('',#11958,#2642);
#2065=LINE('',#11959,#2643);
#2066=LINE('',#11970,#2644);
#2067=LINE('',#11971,#2645);
#2068=LINE('',#11978,#2646);
#2069=LINE('',#11981,#2647);
#2070=LINE('',#11986,#2648);
#2071=LINE('',#11988,#2649);
#2072=LINE('',#11990,#2650);
#2073=LINE('',#11992,#2651);
#2074=LINE('',#11994,#2652);
#2075=LINE('',#11996,#2653);
#2076=LINE('',#11997,#2654);
#2077=LINE('',#11998,#2655);
#2078=LINE('',#12001,#2656);
#2079=LINE('',#12005,#2657);
#2080=LINE('',#12007,#2658);
#2081=LINE('',#12013,#2659);
#2082=LINE('',#12017,#2660);
#2083=LINE('',#12021,#2661);
#2084=LINE('',#12023,#2662);
#2085=LINE('',#12026,#2663);
#2086=LINE('',#12029,#2664);
#2087=LINE('',#12033,#2665);
#2088=LINE('',#12035,#2666);
#2089=LINE('',#12037,#2667);
#2090=LINE('',#12039,#2668);
#2091=LINE('',#12041,#2669);
#2092=LINE('',#12042,#2670);
#2093=LINE('',#12046,#2671);
#2094=LINE('',#12048,#2672);
#2095=LINE('',#12050,#2673);
#2096=LINE('',#12051,#2674);
#2097=LINE('',#12055,#2675);
#2098=LINE('',#12057,#2676);
#2099=LINE('',#12059,#2677);
#2100=LINE('',#12060,#2678);
#2101=LINE('',#12066,#2679);
#2102=LINE('',#12068,#2680);
#2103=LINE('',#12069,#2681);
#2104=LINE('',#12075,#2682);
#2105=LINE('',#12077,#2683);
#2106=LINE('',#12079,#2684);
#2107=LINE('',#12080,#2685);
#2108=LINE('',#12085,#2686);
#2109=LINE('',#12089,#2687);
#2110=LINE('',#12093,#2688);
#2111=LINE('',#12094,#2689);
#2112=LINE('',#12098,#2690);
#2113=LINE('',#12102,#2691);
#2114=LINE('',#12106,#2692);
#2115=LINE('',#12111,#2693);
#2116=LINE('',#12114,#2694);
#2117=LINE('',#12116,#2695);
#2118=LINE('',#12122,#2696);
#2119=LINE('',#12125,#2697);
#2120=LINE('',#12130,#2698);
#2121=LINE('',#12132,#2699);
#2122=LINE('',#12135,#2700);
#2123=LINE('',#12139,#2701);
#2124=LINE('',#12141,#2702);
#2125=LINE('',#12145,#2703);
#2126=LINE('',#12146,#2704);
#2127=LINE('',#12149,#2705);
#2128=LINE('',#12150,#2706);
#2129=LINE('',#12153,#2707);
#2130=LINE('',#12155,#2708);
#2131=LINE('',#12159,#2709);
#2132=LINE('',#12160,#2710);
#2133=LINE('',#12163,#2711);
#2134=LINE('',#12165,#2712);
#2135=LINE('',#12166,#2713);
#2136=LINE('',#12169,#2714);
#2137=LINE('',#12171,#2715);
#2138=LINE('',#12173,#2716);
#2139=LINE('',#12174,#2717);
#2140=LINE('',#12177,#2718);
#2141=LINE('',#12178,#2719);
#2142=LINE('',#12181,#2720);
#2143=LINE('',#12182,#2721);
#2144=LINE('',#12188,#2722);
#2145=LINE('',#12190,#2723);
#2146=LINE('',#12191,#2724);
#2147=LINE('',#12193,#2725);
#2148=LINE('',#12196,#2726);
#2149=LINE('',#12198,#2727);
#2150=LINE('',#12201,#2728);
#2151=LINE('',#12204,#2729);
#2152=LINE('',#12208,#2730);
#2153=LINE('',#12212,#2731);
#2154=LINE('',#12214,#2732);
#2155=LINE('',#12217,#2733);
#2156=LINE('',#12218,#2734);
#2157=LINE('',#12220,#2735);
#2158=LINE('',#12222,#2736);
#2159=LINE('',#12226,#2737);
#2160=LINE('',#12227,#2738);
#2161=LINE('',#12230,#2739);
#2162=LINE('',#12231,#2740);
#2163=LINE('',#12240,#2741);
#2164=LINE('',#12249,#2742);
#2165=LINE('',#12259,#2743);
#2166=LINE('',#12290,#2744);
#2167=LINE('',#12306,#2745);
#2168=LINE('',#12310,#2746);
#2169=LINE('',#12311,#2747);
#2170=LINE('',#12314,#2748);
#2171=LINE('',#12318,#2749);
#2172=LINE('',#12319,#2750);
#2173=LINE('',#12324,#2751);
#2174=LINE('',#12326,#2752);
#2175=LINE('',#12329,#2753);
#2176=LINE('',#12332,#2754);
#2177=LINE('',#12335,#2755);
#2178=LINE('',#12339,#2756);
#2179=LINE('',#12343,#2757);
#2180=LINE('',#12344,#2758);
#2181=LINE('',#12349,#2759);
#2182=LINE('',#12350,#2760);
#2183=LINE('',#12353,#2761);
#2184=LINE('',#12355,#2762);
#2185=LINE('',#12356,#2763);
#2186=LINE('',#12362,#2764);
#2187=LINE('',#12365,#2765);
#2188=LINE('',#12369,#2766);
#2189=LINE('',#12370,#2767);
#2190=LINE('',#12373,#2768);
#2191=LINE('',#12377,#2769);
#2192=LINE('',#12378,#2770);
#2193=LINE('',#12381,#2771);
#2194=LINE('',#12385,#2772);
#2195=LINE('',#12387,#2773);
#2196=LINE('',#12388,#2774);
#2197=LINE('',#12396,#2775);
#2198=LINE('',#12398,#2776);
#2199=LINE('',#12402,#2777);
#2200=LINE('',#12406,#2778);
#2201=LINE('',#12410,#2779);
#2202=LINE('',#12414,#2780);
#2203=LINE('',#12416,#2781);
#2204=LINE('',#12418,#2782);
#2205=LINE('',#12420,#2783);
#2206=LINE('',#12426,#2784);
#2207=LINE('',#12453,#2785);
#2208=LINE('',#12454,#2786);
#2209=LINE('',#12474,#2787);
#2210=LINE('',#12476,#2788);
#2211=LINE('',#12480,#2789);
#2212=LINE('',#12483,#2790);
#2213=LINE('',#12497,#2791);
#2214=LINE('',#12500,#2792);
#2215=LINE('',#12503,#2793);
#2216=LINE('',#12504,#2794);
#2217=LINE('',#12507,#2795);
#2218=LINE('',#12509,#2796);
#2219=LINE('',#12513,#2797);
#2220=LINE('',#12514,#2798);
#2221=LINE('',#12519,#2799);
#2222=LINE('',#12521,#2800);
#2223=LINE('',#12523,#2801);
#2224=LINE('',#12525,#2802);
#2225=LINE('',#12526,#2803);
#2226=LINE('',#12528,#2804);
#2227=LINE('',#12529,#2805);
#2228=LINE('',#12532,#2806);
#2229=LINE('',#12537,#2807);
#2230=LINE('',#12539,#2808);
#2231=LINE('',#12541,#2809);
#2232=LINE('',#12542,#2810);
#2233=LINE('',#12544,#2811);
#2234=LINE('',#12548,#2812);
#2235=LINE('',#12550,#2813);
#2236=LINE('',#12554,#2814);
#2237=LINE('',#12558,#2815);
#2238=LINE('',#12559,#2816);
#2239=LINE('',#12562,#2817);
#2240=LINE('',#12564,#2818);
#2241=LINE('',#12565,#2819);
#2242=LINE('',#12587,#2820);
#2243=LINE('',#12591,#2821);
#2244=LINE('',#12595,#2822);
#2245=LINE('',#12597,#2823);
#2246=LINE('',#12599,#2824);
#2247=LINE('',#12601,#2825);
#2248=LINE('',#12605,#2826);
#2249=LINE('',#12616,#2827);
#2250=LINE('',#12619,#2828);
#2251=LINE('',#12621,#2829);
#2252=LINE('',#12622,#2830);
#2253=LINE('',#12625,#2831);
#2254=LINE('',#12627,#2832);
#2255=LINE('',#12628,#2833);
#2256=LINE('',#12634,#2834);
#2257=LINE('',#12636,#2835);
#2258=LINE('',#12637,#2836);
#2259=LINE('',#12640,#2837);
#2260=LINE('',#12642,#2838);
#2261=LINE('',#12643,#2839);
#2262=LINE('',#12646,#2840);
#2263=LINE('',#12648,#2841);
#2264=LINE('',#12649,#2842);
#2265=LINE('',#12654,#2843);
#2266=LINE('',#12660,#2844);
#2267=LINE('',#12662,#2845);
#2268=LINE('',#12664,#2846);
#2269=LINE('',#12668,#2847);
#2270=LINE('',#12671,#2848);
#2271=LINE('',#12672,#2849);
#2272=LINE('',#12674,#2850);
#2273=LINE('',#12675,#2851);
#2274=LINE('',#12677,#2852);
#2275=LINE('',#12678,#2853);
#2276=LINE('',#12680,#2854);
#2277=LINE('',#12681,#2855);
#2278=LINE('',#12683,#2856);
#2279=LINE('',#12691,#2857);
#2280=LINE('',#12696,#2858);
#2281=LINE('',#12701,#2859);
#2282=LINE('',#12706,#2860);
#2283=LINE('',#12714,#2861);
#2284=LINE('',#12717,#2862);
#2285=LINE('',#12728,#2863);
#2286=LINE('',#12729,#2864);
#2287=LINE('',#12748,#2865);
#2288=LINE('',#12749,#2866);
#2289=LINE('',#12766,#2867);
#2290=LINE('',#12785,#2868);
#2291=LINE('',#12786,#2869);
#2292=LINE('',#12803,#2870);
#2293=LINE('',#12816,#2871);
#2294=LINE('',#12818,#2872);
#2295=LINE('',#12820,#2873);
#2296=LINE('',#12822,#2874);
#2297=LINE('',#12824,#2875);
#2298=LINE('',#12826,#2876);
#2299=LINE('',#12830,#2877);
#2300=LINE('',#12832,#2878);
#2301=LINE('',#12839,#2879);
#2302=LINE('',#12845,#2880);
#2303=LINE('',#12851,#2881);
#2304=LINE('',#12857,#2882);
#2305=LINE('',#12864,#2883);
#2306=LINE('',#12868,#2884);
#2307=LINE('',#12872,#2885);
#2308=LINE('',#12875,#2886);
#2309=LINE('',#12880,#2887);
#2310=LINE('',#12884,#2888);
#2311=LINE('',#12888,#2889);
#2312=LINE('',#12891,#2890);
#2313=LINE('',#12894,#2891);
#2314=LINE('',#12896,#2892);
#2315=LINE('',#12897,#2893);
#2316=LINE('',#12901,#2894);
#2317=LINE('',#12904,#2895);
#2318=LINE('',#12905,#2896);
#2319=LINE('',#12909,#2897);
#2320=LINE('',#12912,#2898);
#2321=LINE('',#12913,#2899);
#2322=LINE('',#12917,#2900);
#2323=LINE('',#12920,#2901);
#2324=LINE('',#12921,#2902);
#2325=LINE('',#12926,#2903);
#2326=LINE('',#12928,#2904);
#2327=LINE('',#12929,#2905);
#2328=LINE('',#12933,#2906);
#2329=LINE('',#12936,#2907);
#2330=LINE('',#12937,#2908);
#2331=LINE('',#12941,#2909);
#2332=LINE('',#12944,#2910);
#2333=LINE('',#12945,#2911);
#2334=LINE('',#12949,#2912);
#2335=LINE('',#12952,#2913);
#2336=LINE('',#12953,#2914);
#2337=LINE('',#12963,#2915);
#2338=LINE('',#12966,#2916);
#2339=LINE('',#12971,#2917);
#2340=LINE('',#12974,#2918);
#2341=LINE('',#12981,#2919);
#2342=LINE('',#12984,#2920);
#2343=LINE('',#12991,#2921);
#2344=LINE('',#12993,#2922);
#2345=LINE('',#13000,#2923);
#2346=LINE('',#13003,#2924);
#2347=LINE('',#13006,#2925);
#2348=LINE('',#13007,#2926);
#2349=LINE('',#13010,#2927);
#2350=LINE('',#13014,#2928);
#2351=LINE('',#13015,#2929);
#2352=LINE('',#13030,#2930);
#2353=LINE('',#13031,#2931);
#2354=LINE('',#13179,#2932);
#2355=LINE('',#13180,#2933);
#2356=LINE('',#13187,#2934);
#2357=LINE('',#13189,#2935);
#2358=LINE('',#13190,#2936);
#2359=LINE('',#13193,#2937);
#2360=LINE('',#13197,#2938);
#2361=LINE('',#13199,#2939);
#2362=LINE('',#13201,#2940);
#2363=LINE('',#13202,#2941);
#2364=LINE('',#13205,#2942);
#2365=LINE('',#13209,#2943);
#2366=LINE('',#13210,#2944);
#2367=LINE('',#13213,#2945);
#2368=LINE('',#13234,#2946);
#2369=LINE('',#13235,#2947);
#2370=LINE('',#13382,#2948);
#2371=LINE('',#13383,#2949);
#2372=LINE('',#13388,#2950);
#2373=LINE('',#13390,#2951);
#2374=LINE('',#13391,#2952);
#2375=LINE('',#13394,#2953);
#2376=LINE('',#13398,#2954);
#2377=LINE('',#13400,#2955);
#2378=LINE('',#13402,#2956);
#2379=LINE('',#13403,#2957);
#2380=LINE('',#13406,#2958);
#2381=LINE('',#13410,#2959);
#2382=LINE('',#13411,#2960);
#2383=LINE('',#13414,#2961);
#2384=LINE('',#13422,#2962);
#2385=LINE('',#13441,#2963);
#2386=LINE('',#13442,#2964);
#2387=LINE('',#13457,#2965);
#2388=LINE('',#13459,#2966);
#2389=LINE('',#13464,#2967);
#2390=LINE('',#13483,#2968);
#2391=LINE('',#13484,#2969);
#2392=LINE('',#13499,#2970);
#2393=LINE('',#13506,#2971);
#2394=LINE('',#13512,#2972);
#2395=LINE('',#13531,#2973);
#2396=LINE('',#13535,#2974);
#2397=LINE('',#13537,#2975);
#2398=LINE('',#13538,#2976);
#2399=LINE('',#13542,#2977);
#2400=LINE('',#13564,#2978);
#2401=LINE('',#13570,#2979);
#2402=LINE('',#13589,#2980);
#2403=LINE('',#13593,#2981);
#2404=LINE('',#13595,#2982);
#2405=LINE('',#13596,#2983);
#2406=LINE('',#13599,#2984);
#2407=LINE('',#13618,#2985);
#2408=LINE('',#13620,#2986);
#2409=LINE('',#13623,#2987);
#2410=LINE('',#13625,#2988);
#2411=LINE('',#13626,#2989);
#2412=LINE('',#13629,#2990);
#2413=LINE('',#13631,#2991);
#2414=LINE('',#13632,#2992);
#2415=LINE('',#13635,#2993);
#2416=LINE('',#13638,#2994);
#2417=LINE('',#13640,#2995);
#2418=LINE('',#13644,#2996);
#2419=LINE('',#13646,#2997);
#2420=LINE('',#13647,#2998);
#2421=LINE('',#13661,#2999);
#2422=LINE('',#13665,#3000);
#2423=LINE('',#13666,#3001);
#2424=LINE('',#13669,#3002);
#2425=LINE('',#13672,#3003);
#2426=LINE('',#13679,#3004);
#2427=LINE('',#13684,#3005);
#2428=LINE('',#13691,#3006);
#2429=LINE('',#13696,#3007);
#2430=LINE('',#13798,#3008);
#2431=LINE('',#13799,#3009);
#2432=LINE('',#13849,#3010);
#2433=LINE('',#13850,#3011);
#2434=LINE('',#13897,#3012);
#2435=LINE('',#13898,#3013);
#2436=LINE('',#13900,#3014);
#2437=LINE('',#13901,#3015);
#2438=LINE('',#13911,#3016);
#2439=LINE('',#14025,#3017);
#2440=LINE('',#14026,#3018);
#2441=LINE('',#14068,#3019);
#2442=LINE('',#14115,#3020);
#2443=LINE('',#14116,#3021);
#2444=LINE('',#14121,#3022);
#2445=LINE('',#14122,#3023);
#2446=LINE('',#14126,#3024);
#2447=LINE('',#14148,#3025);
#2448=LINE('',#14159,#3026);
#2449=LINE('',#14163,#3027);
#2450=LINE('',#14166,#3028);
#2451=LINE('',#14172,#3029);
#2452=LINE('',#14205,#3030);
#2453=LINE('',#14295,#3031);
#2454=LINE('',#14379,#3032);
#2455=LINE('',#14469,#3033);
#2456=LINE('',#14559,#3034);
#2457=LINE('',#14649,#3035);
#2458=LINE('',#14685,#3036);
#2459=LINE('',#14723,#3037);
#2460=LINE('',#14761,#3038);
#2461=LINE('',#14798,#3039);
#2462=LINE('',#16005,#3040);
#2463=LINE('',#16013,#3041);
#2464=LINE('',#16141,#3042);
#2465=LINE('',#16142,#3043);
#2466=LINE('',#16144,#3044);
#2467=LINE('',#16145,#3045);
#2468=LINE('',#16147,#3046);
#2469=LINE('',#16148,#3047);
#2470=LINE('',#16150,#3048);
#2471=LINE('',#16151,#3049);
#2472=LINE('',#16154,#3050);
#2473=LINE('',#16156,#3051);
#2474=LINE('',#16157,#3052);
#2475=LINE('',#16160,#3053);
#2476=LINE('',#16164,#3054);
#2477=LINE('',#16165,#3055);
#2478=LINE('',#16168,#3056);
#2479=LINE('',#16182,#3057);
#2480=LINE('',#16184,#3058);
#2481=LINE('',#16186,#3059);
#2482=LINE('',#16187,#3060);
#2483=LINE('',#16192,#3061);
#2484=LINE('',#16196,#3062);
#2485=LINE('',#16198,#3063);
#2486=LINE('',#16199,#3064);
#2487=LINE('',#16204,#3065);
#2488=LINE('',#16211,#3066);
#2489=LINE('',#16214,#3067);
#2490=LINE('',#16216,#3068);
#2491=LINE('',#16217,#3069);
#2492=LINE('',#16223,#3070);
#2493=LINE('',#16225,#3071);
#2494=LINE('',#16226,#3072);
#2495=LINE('',#16239,#3073);
#2496=LINE('',#16242,#3074);
#2497=LINE('',#16245,#3075);
#2498=LINE('',#16246,#3076);
#2499=LINE('',#16248,#3077);
#2500=LINE('',#16250,#3078);
#2501=LINE('',#16253,#3079);
#2502=LINE('',#16254,#3080);
#2503=LINE('',#16257,#3081);
#2504=LINE('',#16279,#3082);
#2505=LINE('',#16286,#3083);
#2506=LINE('',#16290,#3084);
#2507=LINE('',#16295,#3085);
#2508=LINE('',#16298,#3086);
#2509=LINE('',#16302,#3087);
#2510=LINE('',#16324,#3088);
#2511=LINE('',#16328,#3089);
#2512=LINE('',#16333,#3090);
#2513=LINE('',#16336,#3091);
#2514=LINE('',#16340,#3092);
#2515=LINE('',#16360,#3093);
#2516=LINE('',#16367,#3094);
#2517=LINE('',#16371,#3095);
#2518=LINE('',#16393,#3096);
#2519=LINE('',#16397,#3097);
#2520=LINE('',#16401,#3098);
#2521=LINE('',#16405,#3099);
#2522=LINE('',#16410,#3100);
#2523=LINE('',#16413,#3101);
#2524=LINE('',#16427,#3102);
#2525=LINE('',#16431,#3103);
#2526=LINE('',#16435,#3104);
#2527=LINE('',#16444,#3105);
#2528=LINE('',#16465,#3106);
#2529=LINE('',#16472,#3107);
#2530=LINE('',#16476,#3108);
#2531=LINE('',#16481,#3109);
#2532=LINE('',#16484,#3110);
#2533=LINE('',#16488,#3111);
#2534=LINE('',#16510,#3112);
#2535=LINE('',#16514,#3113);
#2536=LINE('',#16519,#3114);
#2537=LINE('',#16522,#3115);
#2538=LINE('',#16526,#3116);
#2539=LINE('',#16546,#3117);
#2540=LINE('',#16553,#3118);
#2541=LINE('',#16557,#3119);
#2542=LINE('',#16579,#3120);
#2543=LINE('',#16583,#3121);
#2544=LINE('',#16587,#3122);
#2545=LINE('',#16591,#3123);
#2546=LINE('',#16596,#3124);
#2547=LINE('',#16599,#3125);
#2548=LINE('',#16613,#3126);
#2549=LINE('',#16617,#3127);
#2550=LINE('',#16621,#3128);
#2551=LINE('',#16630,#3129);
#2552=LINE('',#16651,#3130);
#2553=LINE('',#16658,#3131);
#2554=LINE('',#16662,#3132);
#2555=LINE('',#16667,#3133);
#2556=LINE('',#16670,#3134);
#2557=LINE('',#16674,#3135);
#2558=LINE('',#16696,#3136);
#2559=LINE('',#16700,#3137);
#2560=LINE('',#16705,#3138);
#2561=LINE('',#16708,#3139);
#2562=LINE('',#16712,#3140);
#2563=LINE('',#16732,#3141);
#2564=LINE('',#16739,#3142);
#2565=LINE('',#16743,#3143);
#2566=LINE('',#16765,#3144);
#2567=LINE('',#16769,#3145);
#2568=LINE('',#16773,#3146);
#2569=LINE('',#16777,#3147);
#2570=LINE('',#16782,#3148);
#2571=LINE('',#16785,#3149);
#2572=LINE('',#16799,#3150);
#2573=LINE('',#16803,#3151);
#2574=LINE('',#16807,#3152);
#2575=LINE('',#16816,#3153);
#2576=LINE('',#16837,#3154);
#2577=LINE('',#16844,#3155);
#2578=LINE('',#16848,#3156);
#2579=LINE('',#16853,#3157);
#2580=LINE('',#16856,#3158);
#2581=LINE('',#16860,#3159);
#2582=LINE('',#16882,#3160);
#2583=LINE('',#16886,#3161);
#2584=LINE('',#16891,#3162);
#2585=LINE('',#16894,#3163);
#2586=LINE('',#16898,#3164);
#2587=LINE('',#16918,#3165);
#2588=LINE('',#16925,#3166);
#2589=LINE('',#16929,#3167);
#2590=LINE('',#16951,#3168);
#2591=LINE('',#16955,#3169);
#2592=LINE('',#16959,#3170);
#2593=LINE('',#16963,#3171);
#2594=LINE('',#16968,#3172);
#2595=LINE('',#16971,#3173);
#2596=LINE('',#16985,#3174);
#2597=LINE('',#16989,#3175);
#2598=LINE('',#16993,#3176);
#2599=LINE('',#17002,#3177);
#2600=VECTOR('',#9257,20.);
#2601=VECTOR('',#9260,20.);
#2602=VECTOR('',#9263,20.);
#2603=VECTOR('',#9268,20.);
#2604=VECTOR('',#9269,20.);
#2605=VECTOR('',#9270,20.);
#2606=VECTOR('',#9273,20.);
#2607=VECTOR('',#9274,20.);
#2608=VECTOR('',#9275,20.);
#2609=VECTOR('',#9276,20.);
#2610=VECTOR('',#9277,20.);
#2611=VECTOR('',#9282,20.);
#2612=VECTOR('',#9285,20.);
#2613=VECTOR('',#9286,20.);
#2614=VECTOR('',#9287,20.);
#2615=VECTOR('',#9292,20.);
#2616=VECTOR('',#9297,20.);
#2617=VECTOR('',#9298,20.);
#2618=VECTOR('',#9299,20.);
#2619=VECTOR('',#9302,20.);
#2620=VECTOR('',#9303,20.);
#2621=VECTOR('',#9304,20.);
#2622=VECTOR('',#9307,20.);
#2623=VECTOR('',#9308,20.);
#2624=VECTOR('',#9309,20.);
#2625=VECTOR('',#9310,20.);
#2626=VECTOR('',#9311,20.);
#2627=VECTOR('',#9314,20.);
#2628=VECTOR('',#9317,20.);
#2629=VECTOR('',#9320,20.);
#2630=VECTOR('',#9321,20.);
#2631=VECTOR('',#9322,20.);
#2632=VECTOR('',#9323,20.);
#2633=VECTOR('',#9328,20.);
#2634=VECTOR('',#9337,20.);
#2635=VECTOR('',#9340,20.);
#2636=VECTOR('',#9343,20.);
#2637=VECTOR('',#9346,20.);
#2638=VECTOR('',#9351,20.);
#2639=VECTOR('',#9354,20.);
#2640=VECTOR('',#9359,20.);
#2641=VECTOR('',#9362,20.);
#2642=VECTOR('',#9373,20.);
#2643=VECTOR('',#9374,20.);
#2644=VECTOR('',#9387,20.);
#2645=VECTOR('',#9388,20.);
#2646=VECTOR('',#9397,20.);
#2647=VECTOR('',#9400,20.);
#2648=VECTOR('',#9407,20.);
#2649=VECTOR('',#9408,20.);
#2650=VECTOR('',#9409,20.);
#2651=VECTOR('',#9410,20.);
#2652=VECTOR('',#9411,20.);
#2653=VECTOR('',#9412,20.);
#2654=VECTOR('',#9413,20.);
#2655=VECTOR('',#9414,20.);
#2656=VECTOR('',#9417,20.);
#2657=VECTOR('',#9422,20.);
#2658=VECTOR('',#9423,20.);
#2659=VECTOR('',#9428,20.);
#2660=VECTOR('',#9431,20.);
#2661=VECTOR('',#9434,20.);
#2662=VECTOR('',#9435,20.);
#2663=VECTOR('',#9438,20.);
#2664=VECTOR('',#9441,20.);
#2665=VECTOR('',#9446,20.);
#2666=VECTOR('',#9447,20.);
#2667=VECTOR('',#9448,20.);
#2668=VECTOR('',#9449,20.);
#2669=VECTOR('',#9450,20.);
#2670=VECTOR('',#9451,20.);
#2671=VECTOR('',#9454,20.);
#2672=VECTOR('',#9455,20.);
#2673=VECTOR('',#9456,20.);
#2674=VECTOR('',#9457,20.);
#2675=VECTOR('',#9460,20.);
#2676=VECTOR('',#9461,20.);
#2677=VECTOR('',#9462,20.);
#2678=VECTOR('',#9463,20.);
#2679=VECTOR('',#9472,20.);
#2680=VECTOR('',#9473,20.);
#2681=VECTOR('',#9474,20.);
#2682=VECTOR('',#9483,20.);
#2683=VECTOR('',#9484,20.);
#2684=VECTOR('',#9485,20.);
#2685=VECTOR('',#9486,20.);
#2686=VECTOR('',#9491,20.);
#2687=VECTOR('',#9494,20.);
#2688=VECTOR('',#9497,20.);
#2689=VECTOR('',#9498,20.);
#2690=VECTOR('',#9501,20.);
#2691=VECTOR('',#9504,20.);
#2692=VECTOR('',#9509,20.);
#2693=VECTOR('',#9514,1.5);
#2694=VECTOR('',#9517,20.);
#2695=VECTOR('',#9518,20.);
#2696=VECTOR('',#9525,1.5);
#2697=VECTOR('',#9528,20.);
#2698=VECTOR('',#9535,1.5);
#2699=VECTOR('',#9536,20.);
#2700=VECTOR('',#9539,20.);
#2701=VECTOR('',#9544,1.5);
#2702=VECTOR('',#9545,20.);
#2703=VECTOR('',#9550,20.);
#2704=VECTOR('',#9551,20.);
#2705=VECTOR('',#9554,20.);
#2706=VECTOR('',#9555,20.);
#2707=VECTOR('',#9558,20.);
#2708=VECTOR('',#9559,20.);
#2709=VECTOR('',#9562,20.);
#2710=VECTOR('',#9563,20.);
#2711=VECTOR('',#9566,20.);
#2712=VECTOR('',#9567,20.);
#2713=VECTOR('',#9568,20.);
#2714=VECTOR('',#9571,20.);
#2715=VECTOR('',#9572,20.);
#2716=VECTOR('',#9573,20.);
#2717=VECTOR('',#9574,20.);
#2718=VECTOR('',#9577,20.);
#2719=VECTOR('',#9578,20.);
#2720=VECTOR('',#9581,20.);
#2721=VECTOR('',#9582,20.);
#2722=VECTOR('',#9587,20.);
#2723=VECTOR('',#9588,20.);
#2724=VECTOR('',#9589,20.);
#2725=VECTOR('',#9590,20.);
#2726=VECTOR('',#9593,20.);
#2727=VECTOR('',#9594,20.);
#2728=VECTOR('',#9597,20.);
#2729=VECTOR('',#9602,20.);
#2730=VECTOR('',#9607,20.);
#2731=VECTOR('',#9612,20.);
#2732=VECTOR('',#9615,20.);
#2733=VECTOR('',#9618,20.);
#2734=VECTOR('',#9619,20.);
#2735=VECTOR('',#9622,20.);
#2736=VECTOR('',#9625,20.);
#2737=VECTOR('',#9630,20.);
#2738=VECTOR('',#9631,20.);
#2739=VECTOR('',#9634,20.);
#2740=VECTOR('',#9635,20.);
#2741=VECTOR('',#9648,20.);
#2742=VECTOR('',#9661,20.);
#2743=VECTOR('',#9674,20.);
#2744=VECTOR('',#9695,20.);
#2745=VECTOR('',#9722,20.);
#2746=VECTOR('',#9727,20.);
#2747=VECTOR('',#9728,20.);
#2748=VECTOR('',#9731,20.);
#2749=VECTOR('',#9736,20.);
#2750=VECTOR('',#9737,20.);
#2751=VECTOR('',#9746,20.);
#2752=VECTOR('',#9749,20.);
#2753=VECTOR('',#9752,1.);
#2754=VECTOR('',#9755,20.);
#2755=VECTOR('',#9758,1.);
#2756=VECTOR('',#9763,20.);
#2757=VECTOR('',#9768,20.);
#2758=VECTOR('',#9769,20.);
#2759=VECTOR('',#9776,20.);
#2760=VECTOR('',#9777,20.);
#2761=VECTOR('',#9780,20.);
#2762=VECTOR('',#9781,20.);
#2763=VECTOR('',#9782,20.);
#2764=VECTOR('',#9791,20.);
#2765=VECTOR('',#9794,20.);
#2766=VECTOR('',#9799,20.);
#2767=VECTOR('',#9800,20.);
#2768=VECTOR('',#9803,20.);
#2769=VECTOR('',#9808,20.);
#2770=VECTOR('',#9809,20.);
#2771=VECTOR('',#9812,20.);
#2772=VECTOR('',#9819,20.);
#2773=VECTOR('',#9822,20.);
#2774=VECTOR('',#9823,20.);
#2775=VECTOR('',#9834,20.);
#2776=VECTOR('',#9835,20.);
#2777=VECTOR('',#9838,20.);
#2778=VECTOR('',#9841,20.);
#2779=VECTOR('',#9844,20.);
#2780=VECTOR('',#9847,20.);
#2781=VECTOR('',#9848,20.);
#2782=VECTOR('',#9849,20.);
#2783=VECTOR('',#9850,20.);
#2784=VECTOR('',#9855,20.);
#2785=VECTOR('',#9874,20.);
#2786=VECTOR('',#9875,20.);
#2787=VECTOR('',#9886,20.);
#2788=VECTOR('',#9887,20.);
#2789=VECTOR('',#9892,20.);
#2790=VECTOR('',#9895,20.);
#2791=VECTOR('',#9902,20.);
#2792=VECTOR('',#9905,20.);
#2793=VECTOR('',#9908,20.);
#2794=VECTOR('',#9909,20.);
#2795=VECTOR('',#9912,20.);
#2796=VECTOR('',#9913,20.);
#2797=VECTOR('',#9918,20.);
#2798=VECTOR('',#9919,20.);
#2799=VECTOR('',#9924,20.);
#2800=VECTOR('',#9925,20.);
#2801=VECTOR('',#9926,20.);
#2802=VECTOR('',#9927,20.);
#2803=VECTOR('',#9928,20.);
#2804=VECTOR('',#9931,20.);
#2805=VECTOR('',#9932,20.);
#2806=VECTOR('',#9935,20.);
#2807=VECTOR('',#9942,20.);
#2808=VECTOR('',#9943,20.);
#2809=VECTOR('',#9944,20.);
#2810=VECTOR('',#9945,20.);
#2811=VECTOR('',#9946,20.);
#2812=VECTOR('',#9949,20.);
#2813=VECTOR('',#9952,20.);
#2814=VECTOR('',#9957,4.);
#2815=VECTOR('',#9962,20.);
#2816=VECTOR('',#9963,20.);
#2817=VECTOR('',#9966,20.);
#2818=VECTOR('',#9967,20.);
#2819=VECTOR('',#9968,20.);
#2820=VECTOR('',#9979,20.);
#2821=VECTOR('',#9982,20.);
#2822=VECTOR('',#9985,20.);
#2823=VECTOR('',#9986,20.);
#2824=VECTOR('',#9987,20.);
#2825=VECTOR('',#9988,20.);
#2826=VECTOR('',#9991,20.);
#2827=VECTOR('',#10002,20.);
#2828=VECTOR('',#10005,20.);
#2829=VECTOR('',#10008,20.);
#2830=VECTOR('',#10009,20.);
#2831=VECTOR('',#10012,20.);
#2832=VECTOR('',#10013,20.);
#2833=VECTOR('',#10014,20.);
#2834=VECTOR('',#10021,20.);
#2835=VECTOR('',#10024,20.);
#2836=VECTOR('',#10025,20.);
#2837=VECTOR('',#10028,20.);
#2838=VECTOR('',#10029,20.);
#2839=VECTOR('',#10030,20.);
#2840=VECTOR('',#10033,20.);
#2841=VECTOR('',#10034,20.);
#2842=VECTOR('',#10035,20.);
#2843=VECTOR('',#10040,20.);
#2844=VECTOR('',#10045,20.);
#2845=VECTOR('',#10046,20.);
#2846=VECTOR('',#10047,20.);
#2847=VECTOR('',#10050,20.);
#2848=VECTOR('',#10055,20.);
#2849=VECTOR('',#10056,20.);
#2850=VECTOR('',#10059,20.);
#2851=VECTOR('',#10060,20.);
#2852=VECTOR('',#10063,20.);
#2853=VECTOR('',#10064,20.);
#2854=VECTOR('',#10067,20.);
#2855=VECTOR('',#10068,20.);
#2856=VECTOR('',#10071,20.);
#2857=VECTOR('',#10084,1.5);
#2858=VECTOR('',#10091,1.5);
#2859=VECTOR('',#10098,1.5);
#2860=VECTOR('',#10105,1.5);
#2861=VECTOR('',#10114,20.);
#2862=VECTOR('',#10117,20.);
#2863=VECTOR('',#10130,20.);
#2864=VECTOR('',#10131,20.);
#2865=VECTOR('',#10142,20.);
#2866=VECTOR('',#10143,20.);
#2867=VECTOR('',#10154,20.);
#2868=VECTOR('',#10165,20.);
#2869=VECTOR('',#10166,20.);
#2870=VECTOR('',#10177,20.);
#2871=VECTOR('',#10184,20.);
#2872=VECTOR('',#10187,20.);
#2873=VECTOR('',#10190,20.);
#2874=VECTOR('',#10193,20.);
#2875=VECTOR('',#10196,20.);
#2876=VECTOR('',#10199,20.);
#2877=VECTOR('',#10206,20.);
#2878=VECTOR('',#10209,20.);
#2879=VECTOR('',#10218,3.20000000000001);
#2880=VECTOR('',#10225,3.20000000000001);
#2881=VECTOR('',#10232,3.2);
#2882=VECTOR('',#10239,3.2);
#2883=VECTOR('',#10246,20.);
#2884=VECTOR('',#10249,20.);
#2885=VECTOR('',#10252,20.);
#2886=VECTOR('',#10255,20.);
#2887=VECTOR('',#10258,20.);
#2888=VECTOR('',#10261,20.);
#2889=VECTOR('',#10264,20.);
#2890=VECTOR('',#10267,20.);
#2891=VECTOR('',#10270,20.);
#2892=VECTOR('',#10271,20.);
#2893=VECTOR('',#10272,20.);
#2894=VECTOR('',#10277,20.);
#2895=VECTOR('',#10280,20.);
#2896=VECTOR('',#10281,20.);
#2897=VECTOR('',#10286,20.);
#2898=VECTOR('',#10289,20.);
#2899=VECTOR('',#10290,20.);
#2900=VECTOR('',#10295,20.);
#2901=VECTOR('',#10298,20.);
#2902=VECTOR('',#10299,20.);
#2903=VECTOR('',#10306,20.);
#2904=VECTOR('',#10307,20.);
#2905=VECTOR('',#10308,20.);
#2906=VECTOR('',#10313,20.);
#2907=VECTOR('',#10316,20.);
#2908=VECTOR('',#10317,20.);
#2909=VECTOR('',#10322,20.);
#2910=VECTOR('',#10325,20.);
#2911=VECTOR('',#10326,20.);
#2912=VECTOR('',#10331,20.);
#2913=VECTOR('',#10334,20.);
#2914=VECTOR('',#10335,20.);
#2915=VECTOR('',#10348,20.);
#2916=VECTOR('',#10351,20.);
#2917=VECTOR('',#10356,20.);
#2918=VECTOR('',#10359,20.);
#2919=VECTOR('',#10368,20.);
#2920=VECTOR('',#10371,20.);
#2921=VECTOR('',#10380,20.);
#2922=VECTOR('',#10383,20.);
#2923=VECTOR('',#10394,20.);
#2924=VECTOR('',#10397,20.);
#2925=VECTOR('',#10400,20.);
#2926=VECTOR('',#10401,20.);
#2927=VECTOR('',#10404,20.);
#2928=VECTOR('',#10409,20.);
#2929=VECTOR('',#10410,20.);
#2930=VECTOR('',#10427,20.);
#2931=VECTOR('',#10428,20.);
#2932=VECTOR('',#10443,20.);
#2933=VECTOR('',#10444,20.);
#2934=VECTOR('',#10453,20.);
#2935=VECTOR('',#10454,20.);
#2936=VECTOR('',#10455,20.);
#2937=VECTOR('',#10458,20.);
#2938=VECTOR('',#10463,20.);
#2939=VECTOR('',#10464,20.);
#2940=VECTOR('',#10465,20.);
#2941=VECTOR('',#10466,20.);
#2942=VECTOR('',#10469,20.);
#2943=VECTOR('',#10474,20.);
#2944=VECTOR('',#10475,20.);
#2945=VECTOR('',#10478,20.);
#2946=VECTOR('',#10503,20.);
#2947=VECTOR('',#10504,20.);
#2948=VECTOR('',#10519,20.);
#2949=VECTOR('',#10520,20.);
#2950=VECTOR('',#10527,20.);
#2951=VECTOR('',#10528,20.);
#2952=VECTOR('',#10529,20.);
#2953=VECTOR('',#10532,20.);
#2954=VECTOR('',#10537,20.);
#2955=VECTOR('',#10538,20.);
#2956=VECTOR('',#10539,20.);
#2957=VECTOR('',#10540,20.);
#2958=VECTOR('',#10543,20.);
#2959=VECTOR('',#10548,20.);
#2960=VECTOR('',#10549,20.);
#2961=VECTOR('',#10552,20.);
#2962=VECTOR('',#10565,20.);
#2963=VECTOR('',#10576,20.);
#2964=VECTOR('',#10577,20.);
#2965=VECTOR('',#10586,20.);
#2966=VECTOR('',#10589,9.);
#2967=VECTOR('',#10596,20.);
#2968=VECTOR('',#10607,20.);
#2969=VECTOR('',#10608,20.);
#2970=VECTOR('',#10617,20.);
#2971=VECTOR('',#10626,20.);
#2972=VECTOR('',#10635,20.);
#2973=VECTOR('',#10646,20.);
#2974=VECTOR('',#10649,20.);
#2975=VECTOR('',#10650,20.);
#2976=VECTOR('',#10651,20.);
#2977=VECTOR('',#10654,20.);
#2978=VECTOR('',#10673,20.);
#2979=VECTOR('',#10682,20.);
#2980=VECTOR('',#10693,20.);
#2981=VECTOR('',#10696,20.);
#2982=VECTOR('',#10697,20.);
#2983=VECTOR('',#10698,20.);
#2984=VECTOR('',#10699,20.);
#2985=VECTOR('',#10716,20.);
#2986=VECTOR('',#10719,20.);
#2987=VECTOR('',#10722,20.);
#2988=VECTOR('',#10723,20.);
#2989=VECTOR('',#10724,20.);
#2990=VECTOR('',#10727,20.);
#2991=VECTOR('',#10728,20.);
#2992=VECTOR('',#10729,20.);
#2993=VECTOR('',#10732,20.);
#2994=VECTOR('',#10735,20.);
#2995=VECTOR('',#10738,20.);
#2996=VECTOR('',#10743,20.);
#2997=VECTOR('',#10744,20.);
#2998=VECTOR('',#10745,20.);
#2999=VECTOR('',#10770,20.);
#3000=VECTOR('',#10775,20.);
#3001=VECTOR('',#10776,20.);
#3002=VECTOR('',#10779,20.);
#3003=VECTOR('',#10784,20.);
#3004=VECTOR('',#10793,7.5);
#3005=VECTOR('',#10800,8.);
#3006=VECTOR('',#10809,7.5);
#3007=VECTOR('',#10816,9.);
#3008=VECTOR('',#10831,20.);
#3009=VECTOR('',#10832,20.);
#3010=VECTOR('',#10839,20.);
#3011=VECTOR('',#10840,20.);
#3012=VECTOR('',#10845,20.);
#3013=VECTOR('',#10846,20.);
#3014=VECTOR('',#10849,20.);
#3015=VECTOR('',#10850,20.);
#3016=VECTOR('',#10863,20.);
#3017=VECTOR('',#10888,20.);
#3018=VECTOR('',#10889,20.);
#3019=VECTOR('',#10896,20.);
#3020=VECTOR('',#10901,20.);
#3021=VECTOR('',#10902,20.);
#3022=VECTOR('',#10911,20.);
#3023=VECTOR('',#10912,20.);
#3024=VECTOR('',#10917,9.);
#3025=VECTOR('',#10948,7.);
#3026=VECTOR('',#10963,5.5);
#3027=VECTOR('',#10968,5.);
#3028=VECTOR('',#10973,4.);
#3029=VECTOR('',#10980,9.);
#3030=VECTOR('',#10985,9.);
#3031=VECTOR('',#10988,9.);
#3032=VECTOR('',#10991,9.);
#3033=VECTOR('',#10994,9.);
#3034=VECTOR('',#10997,9.);
#3035=VECTOR('',#11000,7.4455);
#3036=VECTOR('',#11005,7.4455);
#3037=VECTOR('',#11008,7.4455);
#3038=VECTOR('',#11011,7.4455);
#3039=VECTOR('',#11014,7.4455);
#3040=VECTOR('',#11029,11.);
#3041=VECTOR('',#11040,7.);
#3042=VECTOR('',#11071,20.);
#3043=VECTOR('',#11072,20.);
#3044=VECTOR('',#11075,20.);
#3045=VECTOR('',#11076,20.);
#3046=VECTOR('',#11079,20.);
#3047=VECTOR('',#11080,20.);
#3048=VECTOR('',#11083,20.);
#3049=VECTOR('',#11084,20.);
#3050=VECTOR('',#11087,20.);
#3051=VECTOR('',#11088,20.);
#3052=VECTOR('',#11089,20.);
#3053=VECTOR('',#11092,20.);
#3054=VECTOR('',#11097,20.);
#3055=VECTOR('',#11098,20.);
#3056=VECTOR('',#11101,20.);
#3057=VECTOR('',#11116,20.);
#3058=VECTOR('',#11117,20.);
#3059=VECTOR('',#11118,20.);
#3060=VECTOR('',#11119,20.);
#3061=VECTOR('',#11124,20.);
#3062=VECTOR('',#11129,20.);
#3063=VECTOR('',#11130,20.);
#3064=VECTOR('',#11131,20.);
#3065=VECTOR('',#11136,20.);
#3066=VECTOR('',#11145,20.);
#3067=VECTOR('',#11148,20.);
#3068=VECTOR('',#11149,20.);
#3069=VECTOR('',#11150,20.);
#3070=VECTOR('',#11157,20.);
#3071=VECTOR('',#11160,20.);
#3072=VECTOR('',#11161,20.);
#3073=VECTOR('',#11174,20.);
#3074=VECTOR('',#11177,20.);
#3075=VECTOR('',#11182,20.);
#3076=VECTOR('',#11183,20.);
#3077=VECTOR('',#11186,20.);
#3078=VECTOR('',#11189,20.);
#3079=VECTOR('',#11194,20.);
#3080=VECTOR('',#11195,20.);
#3081=VECTOR('',#11200,20.);
#3082=VECTOR('',#11207,10.);
#3083=VECTOR('',#11214,10.);
#3084=VECTOR('',#11219,10.);
#3085=VECTOR('',#11224,10.);
#3086=VECTOR('',#11227,10.);
#3087=VECTOR('',#11232,10.);
#3088=VECTOR('',#11239,10.);
#3089=VECTOR('',#11244,10.);
#3090=VECTOR('',#11249,10.);
#3091=VECTOR('',#11252,10.);
#3092=VECTOR('',#11257,10.);
#3093=VECTOR('',#11260,10.);
#3094=VECTOR('',#11267,10.);
#3095=VECTOR('',#11272,10.);
#3096=VECTOR('',#11279,10.);
#3097=VECTOR('',#11284,10.);
#3098=VECTOR('',#11289,10.);
#3099=VECTOR('',#11294,10.);
#3100=VECTOR('',#11301,10.);
#3101=VECTOR('',#11306,10.);
#3102=VECTOR('',#11325,0.839230484541328);
#3103=VECTOR('',#11330,0.919615242270664);
#3104=VECTOR('',#11335,1.);
#3105=VECTOR('',#11348,2.11281731799709);
#3106=VECTOR('',#11353,10.);
#3107=VECTOR('',#11360,10.);
#3108=VECTOR('',#11365,10.);
#3109=VECTOR('',#11370,10.);
#3110=VECTOR('',#11373,10.);
#3111=VECTOR('',#11378,10.);
#3112=VECTOR('',#11385,10.);
#3113=VECTOR('',#11390,10.);
#3114=VECTOR('',#11395,10.);
#3115=VECTOR('',#11398,10.);
#3116=VECTOR('',#11403,10.);
#3117=VECTOR('',#11406,10.);
#3118=VECTOR('',#11413,10.);
#3119=VECTOR('',#11418,10.);
#3120=VECTOR('',#11425,10.);
#3121=VECTOR('',#11430,10.);
#3122=VECTOR('',#11435,10.);
#3123=VECTOR('',#11440,10.);
#3124=VECTOR('',#11447,10.);
#3125=VECTOR('',#11452,10.);
#3126=VECTOR('',#11471,0.839230484541328);
#3127=VECTOR('',#11476,0.919615242270664);
#3128=VECTOR('',#11481,1.);
#3129=VECTOR('',#11494,2.11281731799709);
#3130=VECTOR('',#11499,10.);
#3131=VECTOR('',#11506,10.);
#3132=VECTOR('',#11511,10.);
#3133=VECTOR('',#11516,10.);
#3134=VECTOR('',#11519,10.);
#3135=VECTOR('',#11524,10.);
#3136=VECTOR('',#11531,10.);
#3137=VECTOR('',#11536,10.);
#3138=VECTOR('',#11541,10.);
#3139=VECTOR('',#11544,10.);
#3140=VECTOR('',#11549,10.);
#3141=VECTOR('',#11552,10.);
#3142=VECTOR('',#11559,10.);
#3143=VECTOR('',#11564,10.);
#3144=VECTOR('',#11571,10.);
#3145=VECTOR('',#11576,10.);
#3146=VECTOR('',#11581,10.);
#3147=VECTOR('',#11586,10.);
#3148=VECTOR('',#11593,10.);
#3149=VECTOR('',#11598,10.);
#3150=VECTOR('',#11617,0.839230484541328);
#3151=VECTOR('',#11622,0.919615242270664);
#3152=VECTOR('',#11627,1.);
#3153=VECTOR('',#11640,2.11281731799709);
#3154=VECTOR('',#11645,10.);
#3155=VECTOR('',#11652,10.);
#3156=VECTOR('',#11657,10.);
#3157=VECTOR('',#11662,10.);
#3158=VECTOR('',#11665,10.);
#3159=VECTOR('',#11670,10.);
#3160=VECTOR('',#11677,10.);
#3161=VECTOR('',#11682,10.);
#3162=VECTOR('',#11687,10.);
#3163=VECTOR('',#11690,10.);
#3164=VECTOR('',#11695,10.);
#3165=VECTOR('',#11698,10.);
#3166=VECTOR('',#11705,10.);
#3167=VECTOR('',#11710,10.);
#3168=VECTOR('',#11717,10.);
#3169=VECTOR('',#11722,10.);
#3170=VECTOR('',#11727,10.);
#3171=VECTOR('',#11732,10.);
#3172=VECTOR('',#11739,10.);
#3173=VECTOR('',#11744,10.);
#3174=VECTOR('',#11763,0.839230484541328);
#3175=VECTOR('',#11768,0.919615242270664);
#3176=VECTOR('',#11773,1.);
#3177=VECTOR('',#11786,2.11281731799709);
#3178=VERTEX_POINT('',#11814);
#3179=VERTEX_POINT('',#11815);
#3180=VERTEX_POINT('',#11817);
#3181=VERTEX_POINT('',#11830);
#3182=VERTEX_POINT('',#11832);
#3183=VERTEX_POINT('',#11834);
#3184=VERTEX_POINT('',#11836);
#3185=VERTEX_POINT('',#11840);
#3186=VERTEX_POINT('',#11842);
#3187=VERTEX_POINT('',#11846);
#3188=VERTEX_POINT('',#11847);
#3189=VERTEX_POINT('',#11849);
#3190=VERTEX_POINT('',#11852);
#3191=VERTEX_POINT('',#11856);
#3192=VERTEX_POINT('',#11860);
#3193=VERTEX_POINT('',#11862);
#3194=VERTEX_POINT('',#11866);
#3195=VERTEX_POINT('',#11868);
#3196=VERTEX_POINT('',#11872);
#3197=VERTEX_POINT('',#11873);
#3198=VERTEX_POINT('',#11878);
#3199=VERTEX_POINT('',#11880);
#3200=VERTEX_POINT('',#11884);
#3201=VERTEX_POINT('',#11886);
#3202=VERTEX_POINT('',#11888);
#3203=VERTEX_POINT('',#11890);
#3204=VERTEX_POINT('',#11894);
#3205=VERTEX_POINT('',#11896);
#3206=VERTEX_POINT('',#11898);
#3207=VERTEX_POINT('',#11900);
#3208=VERTEX_POINT('',#11902);
#3209=VERTEX_POINT('',#11904);
#3210=VERTEX_POINT('',#11906);
#3211=VERTEX_POINT('',#11908);
#3212=VERTEX_POINT('',#11910);
#3213=VERTEX_POINT('',#11912);
#3214=VERTEX_POINT('',#11914);
#3215=VERTEX_POINT('',#11916);
#3216=VERTEX_POINT('',#11920);
#3217=VERTEX_POINT('',#11921);
#3218=VERTEX_POINT('',#11923);
#3219=VERTEX_POINT('',#11925);
#3220=VERTEX_POINT('',#11929);
#3221=VERTEX_POINT('',#11930);
#3222=VERTEX_POINT('',#11932);
#3223=VERTEX_POINT('',#11934);
#3224=VERTEX_POINT('',#11938);
#3225=VERTEX_POINT('',#11940);
#3226=VERTEX_POINT('',#11944);
#3227=VERTEX_POINT('',#11946);
#3228=VERTEX_POINT('',#11948);
#3229=VERTEX_POINT('',#11952);
#3230=VERTEX_POINT('',#11953);
#3231=VERTEX_POINT('',#11961);
#3232=VERTEX_POINT('',#11962);
#3233=VERTEX_POINT('',#11967);
#3234=VERTEX_POINT('',#11968);
#3235=VERTEX_POINT('',#11975);
#3236=VERTEX_POINT('',#11977);
#3237=VERTEX_POINT('',#11979);
#3238=VERTEX_POINT('',#11985);
#3239=VERTEX_POINT('',#11987);
#3240=VERTEX_POINT('',#11989);
#3241=VERTEX_POINT('',#11991);
#3242=VERTEX_POINT('',#11993);
#3243=VERTEX_POINT('',#11995);
#3244=VERTEX_POINT('',#12000);
#3245=VERTEX_POINT('',#12004);
#3246=VERTEX_POINT('',#12006);
#3247=VERTEX_POINT('',#12008);
#3248=VERTEX_POINT('',#12010);
#3249=VERTEX_POINT('',#12012);
#3250=VERTEX_POINT('',#12014);
#3251=VERTEX_POINT('',#12016);
#3252=VERTEX_POINT('',#12018);
#3253=VERTEX_POINT('',#12020);
#3254=VERTEX_POINT('',#12022);
#3255=VERTEX_POINT('',#12024);
#3256=VERTEX_POINT('',#12028);
#3257=VERTEX_POINT('',#12032);
#3258=VERTEX_POINT('',#12034);
#3259=VERTEX_POINT('',#12036);
#3260=VERTEX_POINT('',#12038);
#3261=VERTEX_POINT('',#12040);
#3262=VERTEX_POINT('',#12044);
#3263=VERTEX_POINT('',#12045);
#3264=VERTEX_POINT('',#12047);
#3265=VERTEX_POINT('',#12049);
#3266=VERTEX_POINT('',#12053);
#3267=VERTEX_POINT('',#12054);
#3268=VERTEX_POINT('',#12056);
#3269=VERTEX_POINT('',#12058);
#3270=VERTEX_POINT('',#12065);
#3271=VERTEX_POINT('',#12067);
#3272=VERTEX_POINT('',#12074);
#3273=VERTEX_POINT('',#12076);
#3274=VERTEX_POINT('',#12078);
#3275=VERTEX_POINT('',#12082);
#3276=VERTEX_POINT('',#12084);
#3277=VERTEX_POINT('',#12086);
#3278=VERTEX_POINT('',#12088);
#3279=VERTEX_POINT('',#12090);
#3280=VERTEX_POINT('',#12092);
#3281=VERTEX_POINT('',#12095);
#3282=VERTEX_POINT('',#12097);
#3283=VERTEX_POINT('',#12099);
#3284=VERTEX_POINT('',#12101);
#3285=VERTEX_POINT('',#12104);
#3286=VERTEX_POINT('',#12108);
#3287=VERTEX_POINT('',#12110);
#3288=VERTEX_POINT('',#12112);
#3289=VERTEX_POINT('',#12115);
#3290=VERTEX_POINT('',#12119);
#3291=VERTEX_POINT('',#12121);
#3292=VERTEX_POINT('',#12123);
#3293=VERTEX_POINT('',#12128);
#3294=VERTEX_POINT('',#12131);
#3295=VERTEX_POINT('',#12133);
#3296=VERTEX_POINT('',#12137);
#3297=VERTEX_POINT('',#12140);
#3298=VERTEX_POINT('',#12144);
#3299=VERTEX_POINT('',#12148);
#3300=VERTEX_POINT('',#12152);
#3301=VERTEX_POINT('',#12154);
#3302=VERTEX_POINT('',#12156);
#3303=VERTEX_POINT('',#12158);
#3304=VERTEX_POINT('',#12162);
#3305=VERTEX_POINT('',#12164);
#3306=VERTEX_POINT('',#12168);
#3307=VERTEX_POINT('',#12170);
#3308=VERTEX_POINT('',#12172);
#3309=VERTEX_POINT('',#12176);
#3310=VERTEX_POINT('',#12180);
#3311=VERTEX_POINT('',#12184);
#3312=VERTEX_POINT('',#12185);
#3313=VERTEX_POINT('',#12187);
#3314=VERTEX_POINT('',#12189);
#3315=VERTEX_POINT('',#12192);
#3316=VERTEX_POINT('',#12194);
#3317=VERTEX_POINT('',#12197);
#3318=VERTEX_POINT('',#12200);
#3319=VERTEX_POINT('',#12206);
#3320=VERTEX_POINT('',#12210);
#3321=VERTEX_POINT('',#12216);
#3322=VERTEX_POINT('',#12225);
#3323=VERTEX_POINT('',#12229);
#3324=VERTEX_POINT('',#12237);
#3325=VERTEX_POINT('',#12239);
#3326=VERTEX_POINT('',#12243);
#3327=VERTEX_POINT('',#12247);
#3328=VERTEX_POINT('',#12251);
#3329=VERTEX_POINT('',#12253);
#3330=VERTEX_POINT('',#12257);
#3331=VERTEX_POINT('',#12287);
#3332=VERTEX_POINT('',#12289);
#3333=VERTEX_POINT('',#12293);
#3334=VERTEX_POINT('',#12305);
#3335=VERTEX_POINT('',#12309);
#3336=VERTEX_POINT('',#12313);
#3337=VERTEX_POINT('',#12317);
#3338=VERTEX_POINT('',#12328);
#3339=VERTEX_POINT('',#12330);
#3340=VERTEX_POINT('',#12334);
#3341=VERTEX_POINT('',#12338);
#3342=VERTEX_POINT('',#12342);
#3343=VERTEX_POINT('',#12348);
#3344=VERTEX_POINT('',#12352);
#3345=VERTEX_POINT('',#12354);
#3346=VERTEX_POINT('',#12360);
#3347=VERTEX_POINT('',#12364);
#3348=VERTEX_POINT('',#12368);
#3349=VERTEX_POINT('',#12372);
#3350=VERTEX_POINT('',#12376);
#3351=VERTEX_POINT('',#12380);
#3352=VERTEX_POINT('',#12394);
#3353=VERTEX_POINT('',#12395);
#3354=VERTEX_POINT('',#12397);
#3355=VERTEX_POINT('',#12399);
#3356=VERTEX_POINT('',#12401);
#3357=VERTEX_POINT('',#12403);
#3358=VERTEX_POINT('',#12405);
#3359=VERTEX_POINT('',#12407);
#3360=VERTEX_POINT('',#12409);
#3361=VERTEX_POINT('',#12411);
#3362=VERTEX_POINT('',#12413);
#3363=VERTEX_POINT('',#12415);
#3364=VERTEX_POINT('',#12417);
#3365=VERTEX_POINT('',#12419);
#3366=VERTEX_POINT('',#12421);
#3367=VERTEX_POINT('',#12423);
#3368=VERTEX_POINT('',#12425);
#3369=VERTEX_POINT('',#12428);
#3370=VERTEX_POINT('',#12430);
#3371=VERTEX_POINT('',#12441);
#3372=VERTEX_POINT('',#12442);
#3373=VERTEX_POINT('',#12444);
#3374=VERTEX_POINT('',#12446);
#3375=VERTEX_POINT('',#12450);
#3376=VERTEX_POINT('',#12451);
#3377=VERTEX_POINT('',#12464);
#3378=VERTEX_POINT('',#12465);
#3379=VERTEX_POINT('',#12467);
#3380=VERTEX_POINT('',#12469);
#3381=VERTEX_POINT('',#12473);
#3382=VERTEX_POINT('',#12475);
#3383=VERTEX_POINT('',#12479);
#3384=VERTEX_POINT('',#12481);
#3385=VERTEX_POINT('',#12496);
#3386=VERTEX_POINT('',#12498);
#3387=VERTEX_POINT('',#12502);
#3388=VERTEX_POINT('',#12506);
#3389=VERTEX_POINT('',#12508);
#3390=VERTEX_POINT('',#12512);
#3391=VERTEX_POINT('',#12515);
#3392=VERTEX_POINT('',#12518);
#3393=VERTEX_POINT('',#12520);
#3394=VERTEX_POINT('',#12522);
#3395=VERTEX_POINT('',#12524);
#3396=VERTEX_POINT('',#12531);
#3397=VERTEX_POINT('',#12536);
#3398=VERTEX_POINT('',#12538);
#3399=VERTEX_POINT('',#12540);
#3400=VERTEX_POINT('',#12543);
#3401=VERTEX_POINT('',#12545);
#3402=VERTEX_POINT('',#12547);
#3403=VERTEX_POINT('',#12552);
#3404=VERTEX_POINT('',#12557);
#3405=VERTEX_POINT('',#12561);
#3406=VERTEX_POINT('',#12563);
#3407=VERTEX_POINT('',#12567);
#3408=VERTEX_POINT('',#12586);
#3409=VERTEX_POINT('',#12588);
#3410=VERTEX_POINT('',#12590);
#3411=VERTEX_POINT('',#12592);
#3412=VERTEX_POINT('',#12594);
#3413=VERTEX_POINT('',#12596);
#3414=VERTEX_POINT('',#12598);
#3415=VERTEX_POINT('',#12600);
#3416=VERTEX_POINT('',#12602);
#3417=VERTEX_POINT('',#12604);
#3418=VERTEX_POINT('',#12607);
#3419=VERTEX_POINT('',#12609);
#3420=VERTEX_POINT('',#12612);
#3421=VERTEX_POINT('',#12613);
#3422=VERTEX_POINT('',#12615);
#3423=VERTEX_POINT('',#12617);
#3424=VERTEX_POINT('',#12624);
#3425=VERTEX_POINT('',#12626);
#3426=VERTEX_POINT('',#12630);
#3427=VERTEX_POINT('',#12632);
#3428=VERTEX_POINT('',#12639);
#3429=VERTEX_POINT('',#12641);
#3430=VERTEX_POINT('',#12645);
#3431=VERTEX_POINT('',#12647);
#3432=VERTEX_POINT('',#12651);
#3433=VERTEX_POINT('',#12653);
#3434=VERTEX_POINT('',#12655);
#3435=VERTEX_POINT('',#12657);
#3436=VERTEX_POINT('',#12659);
#3437=VERTEX_POINT('',#12661);
#3438=VERTEX_POINT('',#12663);
#3439=VERTEX_POINT('',#12665);
#3440=VERTEX_POINT('',#12667);
#3441=VERTEX_POINT('',#12690);
#3442=VERTEX_POINT('',#12695);
#3443=VERTEX_POINT('',#12700);
#3444=VERTEX_POINT('',#12705);
#3445=VERTEX_POINT('',#12710);
#3446=VERTEX_POINT('',#12711);
#3447=VERTEX_POINT('',#12713);
#3448=VERTEX_POINT('',#12715);
#3449=VERTEX_POINT('',#12719);
#3450=VERTEX_POINT('',#12720);
#3451=VERTEX_POINT('',#12725);
#3452=VERTEX_POINT('',#12726);
#3453=VERTEX_POINT('',#12739);
#3454=VERTEX_POINT('',#12740);
#3455=VERTEX_POINT('',#12745);
#3456=VERTEX_POINT('',#12746);
#3457=VERTEX_POINT('',#12759);
#3458=VERTEX_POINT('',#12764);
#3459=VERTEX_POINT('',#12776);
#3460=VERTEX_POINT('',#12777);
#3461=VERTEX_POINT('',#12782);
#3462=VERTEX_POINT('',#12783);
#3463=VERTEX_POINT('',#12796);
#3464=VERTEX_POINT('',#12801);
#3465=VERTEX_POINT('',#12836);
#3466=VERTEX_POINT('',#12838);
#3467=VERTEX_POINT('',#12842);
#3468=VERTEX_POINT('',#12844);
#3469=VERTEX_POINT('',#12848);
#3470=VERTEX_POINT('',#12850);
#3471=VERTEX_POINT('',#12854);
#3472=VERTEX_POINT('',#12856);
#3473=VERTEX_POINT('',#12860);
#3474=VERTEX_POINT('',#12861);
#3475=VERTEX_POINT('',#12863);
#3476=VERTEX_POINT('',#12865);
#3477=VERTEX_POINT('',#12867);
#3478=VERTEX_POINT('',#12869);
#3479=VERTEX_POINT('',#12871);
#3480=VERTEX_POINT('',#12873);
#3481=VERTEX_POINT('',#12876);
#3482=VERTEX_POINT('',#12877);
#3483=VERTEX_POINT('',#12879);
#3484=VERTEX_POINT('',#12881);
#3485=VERTEX_POINT('',#12883);
#3486=VERTEX_POINT('',#12885);
#3487=VERTEX_POINT('',#12887);
#3488=VERTEX_POINT('',#12889);
#3489=VERTEX_POINT('',#12893);
#3490=VERTEX_POINT('',#12895);
#3491=VERTEX_POINT('',#12899);
#3492=VERTEX_POINT('',#12903);
#3493=VERTEX_POINT('',#12907);
#3494=VERTEX_POINT('',#12911);
#3495=VERTEX_POINT('',#12915);
#3496=VERTEX_POINT('',#12919);
#3497=VERTEX_POINT('',#12925);
#3498=VERTEX_POINT('',#12927);
#3499=VERTEX_POINT('',#12931);
#3500=VERTEX_POINT('',#12935);
#3501=VERTEX_POINT('',#12939);
#3502=VERTEX_POINT('',#12943);
#3503=VERTEX_POINT('',#12947);
#3504=VERTEX_POINT('',#12951);
#3505=VERTEX_POINT('',#12959);
#3506=VERTEX_POINT('',#12960);
#3507=VERTEX_POINT('',#12962);
#3508=VERTEX_POINT('',#12964);
#3509=VERTEX_POINT('',#12968);
#3510=VERTEX_POINT('',#12970);
#3511=VERTEX_POINT('',#12972);
#3512=VERTEX_POINT('',#12978);
#3513=VERTEX_POINT('',#12980);
#3514=VERTEX_POINT('',#12982);
#3515=VERTEX_POINT('',#12988);
#3516=VERTEX_POINT('',#12990);
#3517=VERTEX_POINT('',#12999);
#3518=VERTEX_POINT('',#13001);
#3519=VERTEX_POINT('',#13005);
#3520=VERTEX_POINT('',#13009);
#3521=VERTEX_POINT('',#13013);
#3522=VERTEX_POINT('',#13017);
#3523=VERTEX_POINT('',#13020);
#3524=VERTEX_POINT('',#13021);
#3525=VERTEX_POINT('',#13023);
#3526=VERTEX_POINT('',#13027);
#3527=VERTEX_POINT('',#13028);
#3528=VERTEX_POINT('',#13067);
#3529=VERTEX_POINT('',#13068);
#3530=VERTEX_POINT('',#13122);
#3531=VERTEX_POINT('',#13123);
#3532=VERTEX_POINT('',#13162);
#3533=VERTEX_POINT('',#13163);
#3534=VERTEX_POINT('',#13176);
#3535=VERTEX_POINT('',#13177);
#3536=VERTEX_POINT('',#13182);
#3537=VERTEX_POINT('',#13186);
#3538=VERTEX_POINT('',#13188);
#3539=VERTEX_POINT('',#13192);
#3540=VERTEX_POINT('',#13196);
#3541=VERTEX_POINT('',#13198);
#3542=VERTEX_POINT('',#13200);
#3543=VERTEX_POINT('',#13204);
#3544=VERTEX_POINT('',#13208);
#3545=VERTEX_POINT('',#13212);
#3546=VERTEX_POINT('',#13216);
#3547=VERTEX_POINT('',#13218);
#3548=VERTEX_POINT('',#13220);
#3549=VERTEX_POINT('',#13224);
#3550=VERTEX_POINT('',#13225);
#3551=VERTEX_POINT('',#13227);
#3552=VERTEX_POINT('',#13231);
#3553=VERTEX_POINT('',#13232);
#3554=VERTEX_POINT('',#13271);
#3555=VERTEX_POINT('',#13272);
#3556=VERTEX_POINT('',#13326);
#3557=VERTEX_POINT('',#13327);
#3558=VERTEX_POINT('',#13366);
#3559=VERTEX_POINT('',#13367);
#3560=VERTEX_POINT('',#13380);
#3561=VERTEX_POINT('',#13387);
#3562=VERTEX_POINT('',#13389);
#3563=VERTEX_POINT('',#13393);
#3564=VERTEX_POINT('',#13397);
#3565=VERTEX_POINT('',#13399);
#3566=VERTEX_POINT('',#13401);
#3567=VERTEX_POINT('',#13405);
#3568=VERTEX_POINT('',#13409);
#3569=VERTEX_POINT('',#13413);
#3570=VERTEX_POINT('',#13420);
#3571=VERTEX_POINT('',#13432);
#3572=VERTEX_POINT('',#13433);
#3573=VERTEX_POINT('',#13438);
#3574=VERTEX_POINT('',#13439);
#3575=VERTEX_POINT('',#13455);
#3576=VERTEX_POINT('',#13462);
#3577=VERTEX_POINT('',#13474);
#3578=VERTEX_POINT('',#13475);
#3579=VERTEX_POINT('',#13480);
#3580=VERTEX_POINT('',#13481);
#3581=VERTEX_POINT('',#13497);
#3582=VERTEX_POINT('',#13502);
#3583=VERTEX_POINT('',#13504);
#3584=VERTEX_POINT('',#13508);
#3585=VERTEX_POINT('',#13522);
#3586=VERTEX_POINT('',#13523);
#3587=VERTEX_POINT('',#13528);
#3588=VERTEX_POINT('',#13530);
#3589=VERTEX_POINT('',#13532);
#3590=VERTEX_POINT('',#13534);
#3591=VERTEX_POINT('',#13536);
#3592=VERTEX_POINT('',#13539);
#3593=VERTEX_POINT('',#13540);
#3594=VERTEX_POINT('',#13556);
#3595=VERTEX_POINT('',#13560);
#3596=VERTEX_POINT('',#13562);
#3597=VERTEX_POINT('',#13566);
#3598=VERTEX_POINT('',#13580);
#3599=VERTEX_POINT('',#13581);
#3600=VERTEX_POINT('',#13586);
#3601=VERTEX_POINT('',#13588);
#3602=VERTEX_POINT('',#13590);
#3603=VERTEX_POINT('',#13592);
#3604=VERTEX_POINT('',#13594);
#3605=VERTEX_POINT('',#13597);
#3606=VERTEX_POINT('',#13598);
#3607=VERTEX_POINT('',#13614);
#3608=VERTEX_POINT('',#13622);
#3609=VERTEX_POINT('',#13624);
#3610=VERTEX_POINT('',#13628);
#3611=VERTEX_POINT('',#13630);
#3612=VERTEX_POINT('',#13634);
#3613=VERTEX_POINT('',#13636);
#3614=VERTEX_POINT('',#13643);
#3615=VERTEX_POINT('',#13645);
#3616=VERTEX_POINT('',#13660);
#3617=VERTEX_POINT('',#13664);
#3618=VERTEX_POINT('',#13668);
#3619=VERTEX_POINT('',#13676);
#3620=VERTEX_POINT('',#13678);
#3621=VERTEX_POINT('',#13682);
#3622=VERTEX_POINT('',#13686);
#3623=VERTEX_POINT('',#13689);
#3624=VERTEX_POINT('',#13693);
#3625=VERTEX_POINT('',#13728);
#3626=VERTEX_POINT('',#13729);
#3627=VERTEX_POINT('',#13736);
#3628=VERTEX_POINT('',#13738);
#3629=VERTEX_POINT('',#13776);
#3630=VERTEX_POINT('',#13777);
#3631=VERTEX_POINT('',#13784);
#3632=VERTEX_POINT('',#13786);
#3633=VERTEX_POINT('',#13795);
#3634=VERTEX_POINT('',#13796);
#3635=VERTEX_POINT('',#13830);
#3636=VERTEX_POINT('',#13831);
#3637=VERTEX_POINT('',#13846);
#3638=VERTEX_POINT('',#13847);
#3639=VERTEX_POINT('',#13881);
#3640=VERTEX_POINT('',#13882);
#3641=VERTEX_POINT('',#13903);
#3642=VERTEX_POINT('',#13908);
#3643=VERTEX_POINT('',#13910);
#3644=VERTEX_POINT('',#13914);
#3645=VERTEX_POINT('',#13923);
#3646=VERTEX_POINT('',#13956);
#3647=VERTEX_POINT('',#13957);
#3648=VERTEX_POINT('',#13964);
#3649=VERTEX_POINT('',#13966);
#3650=VERTEX_POINT('',#14004);
#3651=VERTEX_POINT('',#14005);
#3652=VERTEX_POINT('',#14012);
#3653=VERTEX_POINT('',#14014);
#3654=VERTEX_POINT('',#14023);
#3655=VERTEX_POINT('',#14057);
#3656=VERTEX_POINT('',#14066);
#3657=VERTEX_POINT('',#14099);
#3658=VERTEX_POINT('',#14100);
#3659=VERTEX_POINT('',#14125);
#3660=VERTEX_POINT('',#14129);
#3661=VERTEX_POINT('',#14134);
#3662=VERTEX_POINT('',#14138);
#3663=VERTEX_POINT('',#14141);
#3664=VERTEX_POINT('',#14145);
#3665=VERTEX_POINT('',#14146);
#3666=VERTEX_POINT('',#14151);
#3667=VERTEX_POINT('',#14155);
#3668=VERTEX_POINT('',#14158);
#3669=VERTEX_POINT('',#14162);
#3670=VERTEX_POINT('',#14170);
#3671=VERTEX_POINT('',#14171);
#3672=VERTEX_POINT('',#14173);
#3673=VERTEX_POINT('',#14190);
#3674=VERTEX_POINT('',#14203);
#3675=VERTEX_POINT('',#14204);
#3676=VERTEX_POINT('',#14293);
#3677=VERTEX_POINT('',#14294);
#3678=VERTEX_POINT('',#14377);
#3679=VERTEX_POINT('',#14378);
#3680=VERTEX_POINT('',#14467);
#3681=VERTEX_POINT('',#14468);
#3682=VERTEX_POINT('',#14557);
#3683=VERTEX_POINT('',#14558);
#3684=VERTEX_POINT('',#14647);
#3685=VERTEX_POINT('',#14648);
#3686=VERTEX_POINT('',#14650);
#3687=VERTEX_POINT('',#14667);
#3688=VERTEX_POINT('',#14683);
#3689=VERTEX_POINT('',#14684);
#3690=VERTEX_POINT('',#14721);
#3691=VERTEX_POINT('',#14722);
#3692=VERTEX_POINT('',#14759);
#3693=VERTEX_POINT('',#14760);
#3694=VERTEX_POINT('',#14796);
#3695=VERTEX_POINT('',#14797);
#3696=VERTEX_POINT('',#15148);
#3697=VERTEX_POINT('',#15286);
#3698=VERTEX_POINT('',#15421);
#3699=VERTEX_POINT('',#15751);
#3700=VERTEX_POINT('',#15999);
#3701=VERTEX_POINT('',#16003);
#3702=VERTEX_POINT('',#16007);
#3703=VERTEX_POINT('',#16010);
#3704=VERTEX_POINT('',#16041);
#3705=VERTEX_POINT('',#16042);
#3706=VERTEX_POINT('',#16044);
#3707=VERTEX_POINT('',#16072);
#3708=VERTEX_POINT('',#16073);
#3709=VERTEX_POINT('',#16075);
#3710=VERTEX_POINT('',#16103);
#3711=VERTEX_POINT('',#16104);
#3712=VERTEX_POINT('',#16106);
#3713=VERTEX_POINT('',#16134);
#3714=VERTEX_POINT('',#16135);
#3715=VERTEX_POINT('',#16137);
#3716=VERTEX_POINT('',#16153);
#3717=VERTEX_POINT('',#16155);
#3718=VERTEX_POINT('',#16159);
#3719=VERTEX_POINT('',#16163);
#3720=VERTEX_POINT('',#16167);
#3721=VERTEX_POINT('',#16171);
#3722=VERTEX_POINT('',#16172);
#3723=VERTEX_POINT('',#16174);
#3724=VERTEX_POINT('',#16176);
#3725=VERTEX_POINT('',#16180);
#3726=VERTEX_POINT('',#16181);
#3727=VERTEX_POINT('',#16183);
#3728=VERTEX_POINT('',#16185);
#3729=VERTEX_POINT('',#16189);
#3730=VERTEX_POINT('',#16191);
#3731=VERTEX_POINT('',#16195);
#3732=VERTEX_POINT('',#16197);
#3733=VERTEX_POINT('',#16201);
#3734=VERTEX_POINT('',#16203);
#3735=VERTEX_POINT('',#16207);
#3736=VERTEX_POINT('',#16209);
#3737=VERTEX_POINT('',#16213);
#3738=VERTEX_POINT('',#16215);
#3739=VERTEX_POINT('',#16219);
#3740=VERTEX_POINT('',#16221);
#3741=VERTEX_POINT('',#16228);
#3742=VERTEX_POINT('',#16229);
#3743=VERTEX_POINT('',#16231);
#3744=VERTEX_POINT('',#16233);
#3745=VERTEX_POINT('',#16237);
#3746=VERTEX_POINT('',#16238);
#3747=VERTEX_POINT('',#16241);
#3748=VERTEX_POINT('',#16261);
#3749=VERTEX_POINT('',#16262);
#3750=VERTEX_POINT('',#16278);
#3751=VERTEX_POINT('',#16280);
#3752=VERTEX_POINT('',#16282);
#3753=VERTEX_POINT('',#16284);
#3754=VERTEX_POINT('',#16288);
#3755=VERTEX_POINT('',#16292);
#3756=VERTEX_POINT('',#16294);
#3757=VERTEX_POINT('',#16296);
#3758=VERTEX_POINT('',#16300);
#3759=VERTEX_POINT('',#16304);
#3760=VERTEX_POINT('',#16320);
#3761=VERTEX_POINT('',#16322);
#3762=VERTEX_POINT('',#16326);
#3763=VERTEX_POINT('',#16330);
#3764=VERTEX_POINT('',#16332);
#3765=VERTEX_POINT('',#16334);
#3766=VERTEX_POINT('',#16338);
#3767=VERTEX_POINT('',#16342);
#3768=VERTEX_POINT('',#16343);
#3769=VERTEX_POINT('',#16359);
#3770=VERTEX_POINT('',#16361);
#3771=VERTEX_POINT('',#16363);
#3772=VERTEX_POINT('',#16365);
#3773=VERTEX_POINT('',#16369);
#3774=VERTEX_POINT('',#16373);
#3775=VERTEX_POINT('',#16389);
#3776=VERTEX_POINT('',#16391);
#3777=VERTEX_POINT('',#16395);
#3778=VERTEX_POINT('',#16399);
#3779=VERTEX_POINT('',#16403);
#3780=VERTEX_POINT('',#16408);
#3781=VERTEX_POINT('',#16416);
#3782=VERTEX_POINT('',#16418);
#3783=VERTEX_POINT('',#16422);
#3784=VERTEX_POINT('',#16425);
#3785=VERTEX_POINT('',#16429);
#3786=VERTEX_POINT('',#16433);
#3787=VERTEX_POINT('',#16438);
#3788=VERTEX_POINT('',#16440);
#3789=VERTEX_POINT('',#16447);
#3790=VERTEX_POINT('',#16448);
#3791=VERTEX_POINT('',#16464);
#3792=VERTEX_POINT('',#16466);
#3793=VERTEX_POINT('',#16468);
#3794=VERTEX_POINT('',#16470);
#3795=VERTEX_POINT('',#16474);
#3796=VERTEX_POINT('',#16478);
#3797=VERTEX_POINT('',#16480);
#3798=VERTEX_POINT('',#16482);
#3799=VERTEX_POINT('',#16486);
#3800=VERTEX_POINT('',#16490);
#3801=VERTEX_POINT('',#16506);
#3802=VERTEX_POINT('',#16508);
#3803=VERTEX_POINT('',#16512);
#3804=VERTEX_POINT('',#16516);
#3805=VERTEX_POINT('',#16518);
#3806=VERTEX_POINT('',#16520);
#3807=VERTEX_POINT('',#16524);
#3808=VERTEX_POINT('',#16528);
#3809=VERTEX_POINT('',#16529);
#3810=VERTEX_POINT('',#16545);
#3811=VERTEX_POINT('',#16547);
#3812=VERTEX_POINT('',#16549);
#3813=VERTEX_POINT('',#16551);
#3814=VERTEX_POINT('',#16555);
#3815=VERTEX_POINT('',#16559);
#3816=VERTEX_POINT('',#16575);
#3817=VERTEX_POINT('',#16577);
#3818=VERTEX_POINT('',#16581);
#3819=VERTEX_POINT('',#16585);
#3820=VERTEX_POINT('',#16589);
#3821=VERTEX_POINT('',#16594);
#3822=VERTEX_POINT('',#16602);
#3823=VERTEX_POINT('',#16604);
#3824=VERTEX_POINT('',#16608);
#3825=VERTEX_POINT('',#16611);
#3826=VERTEX_POINT('',#16615);
#3827=VERTEX_POINT('',#16619);
#3828=VERTEX_POINT('',#16624);
#3829=VERTEX_POINT('',#16626);
#3830=VERTEX_POINT('',#16633);
#3831=VERTEX_POINT('',#16634);
#3832=VERTEX_POINT('',#16650);
#3833=VERTEX_POINT('',#16652);
#3834=VERTEX_POINT('',#16654);
#3835=VERTEX_POINT('',#16656);
#3836=VERTEX_POINT('',#16660);
#3837=VERTEX_POINT('',#16664);
#3838=VERTEX_POINT('',#16666);
#3839=VERTEX_POINT('',#16668);
#3840=VERTEX_POINT('',#16672);
#3841=VERTEX_POINT('',#16676);
#3842=VERTEX_POINT('',#16692);
#3843=VERTEX_POINT('',#16694);
#3844=VERTEX_POINT('',#16698);
#3845=VERTEX_POINT('',#16702);
#3846=VERTEX_POINT('',#16704);
#3847=VERTEX_POINT('',#16706);
#3848=VERTEX_POINT('',#16710);
#3849=VERTEX_POINT('',#16714);
#3850=VERTEX_POINT('',#16715);
#3851=VERTEX_POINT('',#16731);
#3852=VERTEX_POINT('',#16733);
#3853=VERTEX_POINT('',#16735);
#3854=VERTEX_POINT('',#16737);
#3855=VERTEX_POINT('',#16741);
#3856=VERTEX_POINT('',#16745);
#3857=VERTEX_POINT('',#16761);
#3858=VERTEX_POINT('',#16763);
#3859=VERTEX_POINT('',#16767);
#3860=VERTEX_POINT('',#16771);
#3861=VERTEX_POINT('',#16775);
#3862=VERTEX_POINT('',#16780);
#3863=VERTEX_POINT('',#16788);
#3864=VERTEX_POINT('',#16790);
#3865=VERTEX_POINT('',#16794);
#3866=VERTEX_POINT('',#16797);
#3867=VERTEX_POINT('',#16801);
#3868=VERTEX_POINT('',#16805);
#3869=VERTEX_POINT('',#16810);
#3870=VERTEX_POINT('',#16812);
#3871=VERTEX_POINT('',#16819);
#3872=VERTEX_POINT('',#16820);
#3873=VERTEX_POINT('',#16836);
#3874=VERTEX_POINT('',#16838);
#3875=VERTEX_POINT('',#16840);
#3876=VERTEX_POINT('',#16842);
#3877=VERTEX_POINT('',#16846);
#3878=VERTEX_POINT('',#16850);
#3879=VERTEX_POINT('',#16852);
#3880=VERTEX_POINT('',#16854);
#3881=VERTEX_POINT('',#16858);
#3882=VERTEX_POINT('',#16862);
#3883=VERTEX_POINT('',#16878);
#3884=VERTEX_POINT('',#16880);
#3885=VERTEX_POINT('',#16884);
#3886=VERTEX_POINT('',#16888);
#3887=VERTEX_POINT('',#16890);
#3888=VERTEX_POINT('',#16892);
#3889=VERTEX_POINT('',#16896);
#3890=VERTEX_POINT('',#16900);
#3891=VERTEX_POINT('',#16901);
#3892=VERTEX_POINT('',#16917);
#3893=VERTEX_POINT('',#16919);
#3894=VERTEX_POINT('',#16921);
#3895=VERTEX_POINT('',#16923);
#3896=VERTEX_POINT('',#16927);
#3897=VERTEX_POINT('',#16931);
#3898=VERTEX_POINT('',#16947);
#3899=VERTEX_POINT('',#16949);
#3900=VERTEX_POINT('',#16953);
#3901=VERTEX_POINT('',#16957);
#3902=VERTEX_POINT('',#16961);
#3903=VERTEX_POINT('',#16966);
#3904=VERTEX_POINT('',#16974);
#3905=VERTEX_POINT('',#16976);
#3906=VERTEX_POINT('',#16980);
#3907=VERTEX_POINT('',#16983);
#3908=VERTEX_POINT('',#16987);
#3909=VERTEX_POINT('',#16991);
#3910=VERTEX_POINT('',#16996);
#3911=VERTEX_POINT('',#16998);
#3912=EDGE_CURVE('',#3178,#3179,#2022,.T.);
#3913=EDGE_CURVE('',#3179,#3180,#1950,.T.);
#3914=EDGE_CURVE('',#3180,#3181,#1470,.T.);
#3915=EDGE_CURVE('',#3182,#3181,#2023,.T.);
#3916=EDGE_CURVE('',#3182,#3183,#1471,.F.);
#3917=EDGE_CURVE('',#3183,#3184,#2024,.T.);
#3918=EDGE_CURVE('',#3178,#3184,#1472,.T.);
#3919=EDGE_CURVE('',#3181,#3185,#2025,.T.);
#3920=EDGE_CURVE('',#3185,#3186,#2026,.T.);
#3921=EDGE_CURVE('',#3186,#3182,#2027,.F.);
#3922=EDGE_CURVE('',#3187,#3188,#2028,.T.);
#3923=EDGE_CURVE('',#3189,#3187,#2029,.T.);
#3924=EDGE_CURVE('',#3189,#3179,#2030,.T.);
#3925=EDGE_CURVE('',#3190,#3178,#2031,.T.);
#3926=EDGE_CURVE('',#3188,#3190,#2032,.T.);
#3927=EDGE_CURVE('',#3191,#3189,#1473,.T.);
#3928=EDGE_CURVE('',#3191,#3180,#2033,.T.);
#3929=EDGE_CURVE('',#3192,#3191,#2034,.T.);
#3930=EDGE_CURVE('',#3192,#3193,#2035,.T.);
#3931=EDGE_CURVE('',#3185,#3193,#2036,.T.);
#3932=EDGE_CURVE('',#3194,#3192,#1474,.T.);
#3933=EDGE_CURVE('',#3194,#3195,#2037,.T.);
#3934=EDGE_CURVE('',#3193,#3195,#1475,.T.);
#3935=EDGE_CURVE('',#3196,#3197,#2038,.T.);
#3936=EDGE_CURVE('',#3195,#3196,#2039,.T.);
#3937=EDGE_CURVE('',#3197,#3194,#2040,.T.);
#3938=EDGE_CURVE('',#3198,#3190,#2041,.F.);
#3939=EDGE_CURVE('',#3198,#3199,#2042,.T.);
#3940=EDGE_CURVE('',#3188,#3199,#2043,.T.);
#3941=EDGE_CURVE('',#3200,#3196,#2044,.T.);
#3942=EDGE_CURVE('',#3200,#3201,#2045,.T.);
#3943=EDGE_CURVE('',#3202,#3201,#2046,.F.);
#3944=EDGE_CURVE('',#3203,#3202,#2047,.T.);
#3945=EDGE_CURVE('',#3203,#3186,#2048,.T.);
#3946=EDGE_CURVE('',#3204,#3197,#2049,.T.);
#3947=EDGE_CURVE('',#3205,#3204,#1476,.T.);
#3948=EDGE_CURVE('',#3206,#3205,#2050,.T.);
#3949=EDGE_CURVE('',#3207,#3206,#1477,.T.);
#3950=EDGE_CURVE('',#3208,#3207,#2051,.T.);
#3951=EDGE_CURVE('',#3208,#3209,#2052,.T.);
#3952=EDGE_CURVE('',#3209,#3210,#2053,.T.);
#3953=EDGE_CURVE('',#3210,#3211,#2054,.T.);
#3954=EDGE_CURVE('',#3211,#3212,#1478,.T.);
#3955=EDGE_CURVE('',#3212,#3213,#1479,.T.);
#3956=EDGE_CURVE('',#3213,#3214,#2055,.T.);
#3957=EDGE_CURVE('',#3214,#3215,#1480,.T.);
#3958=EDGE_CURVE('',#3215,#3200,#1481,.T.);
#3959=EDGE_CURVE('',#3216,#3217,#1482,.T.);
#3960=EDGE_CURVE('',#3217,#3218,#2056,.T.);
#3961=EDGE_CURVE('',#3218,#3219,#1483,.F.);
#3962=EDGE_CURVE('',#3219,#3216,#2057,.T.);
#3963=EDGE_CURVE('',#3220,#3221,#2058,.T.);
#3964=EDGE_CURVE('',#3221,#3222,#1484,.T.);
#3965=EDGE_CURVE('',#3222,#3223,#2059,.T.);
#3966=EDGE_CURVE('',#3223,#3220,#237,.T.);
#3967=EDGE_CURVE('',#3223,#3224,#2060,.T.);
#3968=EDGE_CURVE('',#3224,#3225,#238,.T.);
#3969=EDGE_CURVE('',#3225,#3220,#2061,.T.);
#3970=EDGE_CURVE('',#3226,#3216,#1485,.T.);
#3971=EDGE_CURVE('',#3216,#3227,#2062,.T.);
#3972=EDGE_CURVE('',#3227,#3228,#1486,.T.);
#3973=EDGE_CURVE('',#3228,#3226,#2063,.T.);
#3974=EDGE_CURVE('',#3229,#3230,#1487,.T.);
#3975=EDGE_CURVE('',#3230,#3228,#1488,.T.);
#3976=EDGE_CURVE('',#3227,#3229,#1489,.T.);
#3977=EDGE_CURVE('',#3224,#3230,#2064,.T.);
#3978=EDGE_CURVE('',#3229,#3225,#2065,.T.);
#3979=EDGE_CURVE('',#3231,#3232,#1490,.T.);
#3980=EDGE_CURVE('',#3232,#3222,#1491,.T.);
#3981=EDGE_CURVE('',#3221,#3231,#1492,.T.);
#3982=EDGE_CURVE('',#3233,#3234,#1493,.T.);
#3983=EDGE_CURVE('',#3234,#3232,#2066,.T.);
#3984=EDGE_CURVE('',#3231,#3233,#2067,.T.);
#3985=EDGE_CURVE('',#3226,#3217,#1494,.T.);
#3986=EDGE_CURVE('',#3235,#3233,#1495,.T.);
#3987=EDGE_CURVE('',#3233,#3236,#2068,.T.);
#3988=EDGE_CURVE('',#3236,#3237,#1496,.F.);
#3989=EDGE_CURVE('',#3237,#3235,#2069,.T.);
#3990=EDGE_CURVE('',#3235,#3234,#1497,.T.);
#3991=EDGE_CURVE('',#3238,#3218,#2070,.T.);
#3992=EDGE_CURVE('',#3239,#3217,#2071,.T.);
#3993=EDGE_CURVE('',#3240,#3239,#2072,.T.);
#3994=EDGE_CURVE('',#3240,#3241,#2073,.T.);
#3995=EDGE_CURVE('',#3242,#3241,#2074,.T.);
#3996=EDGE_CURVE('',#3243,#3242,#2075,.T.);
#3997=EDGE_CURVE('',#3206,#3243,#2076,.T.);
#3998=EDGE_CURVE('',#3205,#3238,#2077,.T.);
#3999=EDGE_CURVE('',#3226,#3244,#2078,.T.);
#4000=EDGE_CURVE('',#3244,#3239,#1498,.T.);
#4001=EDGE_CURVE('',#3245,#3234,#2079,.T.);
#4002=EDGE_CURVE('',#3246,#3245,#2080,.T.);
#4003=EDGE_CURVE('',#3247,#3246,#1499,.T.);
#4004=EDGE_CURVE('',#3248,#3247,#1500,.T.);
#4005=EDGE_CURVE('',#3249,#3248,#2081,.T.);
#4006=EDGE_CURVE('',#3250,#3249,#1501,.T.);
#4007=EDGE_CURVE('',#3251,#3250,#2082,.T.);
#4008=EDGE_CURVE('',#3252,#3251,#1502,.T.);
#4009=EDGE_CURVE('',#3253,#3252,#2083,.T.);
#4010=EDGE_CURVE('',#3254,#3253,#2084,.T.);
#4011=EDGE_CURVE('',#3255,#3254,#1503,.T.);
#4012=EDGE_CURVE('',#3244,#3255,#2085,.T.);
#4013=EDGE_CURVE('',#3235,#3256,#2086,.T.);
#4014=EDGE_CURVE('',#3256,#3245,#1504,.T.);
#4015=EDGE_CURVE('',#3237,#3257,#2087,.T.);
#4016=EDGE_CURVE('',#3258,#3257,#2088,.T.);
#4017=EDGE_CURVE('',#3258,#3259,#2089,.T.);
#4018=EDGE_CURVE('',#3259,#3260,#2090,.T.);
#4019=EDGE_CURVE('',#3260,#3261,#2091,.T.);
#4020=EDGE_CURVE('',#3256,#3261,#2092,.T.);
#4021=EDGE_CURVE('',#3262,#3263,#2093,.T.);
#4022=EDGE_CURVE('',#3264,#3262,#2094,.T.);
#4023=EDGE_CURVE('',#3265,#3264,#2095,.T.);
#4024=EDGE_CURVE('',#3263,#3265,#2096,.T.);
#4025=EDGE_CURVE('',#3266,#3267,#2097,.T.);
#4026=EDGE_CURVE('',#3268,#3266,#2098,.T.);
#4027=EDGE_CURVE('',#3269,#3268,#2099,.T.);
#4028=EDGE_CURVE('',#3269,#3267,#2100,.T.);
#4029=EDGE_CURVE('',#3267,#3262,#1505,.T.);
#4030=EDGE_CURVE('',#3264,#3269,#1506,.T.);
#4031=EDGE_CURVE('',#3209,#3270,#2101,.T.);
#4032=EDGE_CURVE('',#3271,#3208,#2102,.T.);
#4033=EDGE_CURVE('',#3271,#3270,#2103,.T.);
#4034=EDGE_CURVE('',#3270,#3266,#1507,.T.);
#4035=EDGE_CURVE('',#3268,#3271,#1508,.T.);
#4036=EDGE_CURVE('',#3272,#3207,#2104,.T.);
#4037=EDGE_CURVE('',#3273,#3272,#2105,.T.);
#4038=EDGE_CURVE('',#3274,#3273,#2106,.T.);
#4039=EDGE_CURVE('',#3274,#3265,#2107,.T.);
#4040=EDGE_CURVE('',#3199,#3275,#1509,.T.);
#4041=EDGE_CURVE('',#3275,#3276,#2108,.T.);
#4042=EDGE_CURVE('',#3276,#3277,#1510,.T.);
#4043=EDGE_CURVE('',#3277,#3278,#2109,.T.);
#4044=EDGE_CURVE('',#3278,#3279,#1511,.T.);
#4045=EDGE_CURVE('',#3279,#3280,#2110,.T.);
#4046=EDGE_CURVE('',#3280,#3263,#2111,.T.);
#4047=EDGE_CURVE('',#3281,#3274,#1512,.T.);
#4048=EDGE_CURVE('',#3282,#3281,#2112,.T.);
#4049=EDGE_CURVE('',#3283,#3282,#1513,.T.);
#4050=EDGE_CURVE('',#3284,#3283,#2113,.T.);
#4051=EDGE_CURVE('',#3259,#3284,#1514,.T.);
#4052=EDGE_CURVE('',#3285,#3258,#1515,.T.);
#4053=EDGE_CURVE('',#3187,#3285,#2114,.T.);
#4054=EDGE_CURVE('',#3286,#3286,#1516,.T.);
#4055=EDGE_CURVE('',#3286,#3287,#2115,.T.);
#4056=EDGE_CURVE('',#3288,#3287,#1517,.T.);
#4057=EDGE_CURVE('',#3277,#3288,#2116,.T.);
#4058=EDGE_CURVE('',#3289,#3276,#2117,.T.);
#4059=EDGE_CURVE('',#3287,#3289,#1518,.T.);
#4060=EDGE_CURVE('',#3290,#3290,#1519,.T.);
#4061=EDGE_CURVE('',#3290,#3291,#2118,.T.);
#4062=EDGE_CURVE('',#3292,#3291,#1520,.T.);
#4063=EDGE_CURVE('',#3275,#3292,#2119,.T.);
#4064=EDGE_CURVE('',#3291,#3198,#1521,.T.);
#4065=EDGE_CURVE('',#3293,#3293,#1522,.T.);
#4066=EDGE_CURVE('',#3293,#3212,#2120,.T.);
#4067=EDGE_CURVE('',#3294,#3211,#2121,.T.);
#4068=EDGE_CURVE('',#3295,#3294,#1523,.T.);
#4069=EDGE_CURVE('',#3213,#3295,#2122,.T.);
#4070=EDGE_CURVE('',#3296,#3296,#1524,.T.);
#4071=EDGE_CURVE('',#3296,#3215,#2123,.T.);
#4072=EDGE_CURVE('',#3297,#3214,#2124,.T.);
#4073=EDGE_CURVE('',#3201,#3297,#1525,.T.);
#4074=EDGE_CURVE('',#3288,#3298,#2125,.T.);
#4075=EDGE_CURVE('',#3278,#3298,#2126,.T.);
#4076=EDGE_CURVE('',#3184,#3299,#2127,.T.);
#4077=EDGE_CURVE('',#3299,#3292,#2128,.T.);
#4078=EDGE_CURVE('',#3294,#3300,#2129,.T.);
#4079=EDGE_CURVE('',#3300,#3301,#2130,.T.);
#4080=EDGE_CURVE('',#3301,#3302,#1526,.T.);
#4081=EDGE_CURVE('',#3302,#3303,#2131,.T.);
#4082=EDGE_CURVE('',#3303,#3295,#2132,.T.);
#4083=EDGE_CURVE('',#3210,#3304,#2133,.T.);
#4084=EDGE_CURVE('',#3305,#3304,#2134,.T.);
#4085=EDGE_CURVE('',#3300,#3305,#2135,.T.);
#4086=EDGE_CURVE('',#3303,#3306,#2136,.T.);
#4087=EDGE_CURVE('',#3307,#3306,#2137,.T.);
#4088=EDGE_CURVE('',#3308,#3307,#2138,.F.);
#4089=EDGE_CURVE('',#3297,#3308,#2139,.T.);
#4090=EDGE_CURVE('',#3309,#3305,#2140,.T.);
#4091=EDGE_CURVE('',#3309,#3301,#2141,.T.);
#4092=EDGE_CURVE('',#3280,#3310,#2142,.T.);
#4093=EDGE_CURVE('',#3304,#3310,#2143,.T.);
#4094=EDGE_CURVE('',#3311,#3312,#1527,.T.);
#4095=EDGE_CURVE('',#3312,#3313,#2144,.T.);
#4096=EDGE_CURVE('',#3313,#3314,#2145,.T.);
#4097=EDGE_CURVE('',#3183,#3314,#2146,.F.);
#4098=EDGE_CURVE('',#3315,#3203,#2147,.F.);
#4099=EDGE_CURVE('',#3316,#3315,#1528,.F.);
#4100=EDGE_CURVE('',#3307,#3316,#2148,.F.);
#4101=EDGE_CURVE('',#3306,#3317,#2149,.T.);
#4102=EDGE_CURVE('',#3317,#3309,#1529,.T.);
#4103=EDGE_CURVE('',#3310,#3318,#2150,.T.);
#4104=EDGE_CURVE('',#3318,#3311,#1530,.T.);
#4105=EDGE_CURVE('',#3279,#3318,#2151,.T.);
#4106=EDGE_CURVE('',#3298,#3319,#1531,.F.);
#4107=EDGE_CURVE('',#3319,#3311,#2152,.T.);
#4108=EDGE_CURVE('',#3320,#3319,#1532,.T.);
#4109=EDGE_CURVE('',#3312,#3320,#2153,.T.);
#4110=EDGE_CURVE('',#3317,#3302,#2154,.T.);
#4111=EDGE_CURVE('',#3321,#3320,#2155,.T.);
#4112=EDGE_CURVE('',#3321,#3313,#2156,.T.);
#4113=EDGE_CURVE('',#3289,#3321,#2157,.T.);
#4114=EDGE_CURVE('',#3314,#3299,#2158,.F.);
#4115=EDGE_CURVE('',#3316,#3322,#2159,.T.);
#4116=EDGE_CURVE('',#3308,#3322,#2160,.T.);
#4117=EDGE_CURVE('',#3323,#3202,#2161,.T.);
#4118=EDGE_CURVE('',#3315,#3323,#2162,.T.);
#4119=EDGE_CURVE('',#3322,#3323,#1533,.T.);
#4120=EDGE_CURVE('',#3253,#3324,#1534,.T.);
#4121=EDGE_CURVE('',#3324,#3325,#2163,.T.);
#4122=EDGE_CURVE('',#3325,#3254,#1535,.T.);
#4123=EDGE_CURVE('',#3326,#3255,#1536,.T.);
#4124=EDGE_CURVE('',#3325,#3326,#1537,.T.);
#4125=EDGE_CURVE('',#3327,#3244,#1538,.T.);
#4126=EDGE_CURVE('',#3326,#3327,#2164,.T.);
#4127=EDGE_CURVE('',#3247,#3328,#1539,.T.);
#4128=EDGE_CURVE('',#3328,#3329,#1540,.T.);
#4129=EDGE_CURVE('',#3329,#3248,#1541,.T.);
#4130=EDGE_CURVE('',#3330,#3249,#1542,.T.);
#4131=EDGE_CURVE('',#3329,#3330,#2165,.T.);
#4132=EDGE_CURVE('',#3273,#3250,#1543,.T.);
#4133=EDGE_CURVE('',#3330,#3273,#1544,.T.);
#4134=EDGE_CURVE('',#3272,#3251,#1545,.T.);
#4135=EDGE_CURVE('',#3243,#3252,#1546,.T.);
#4136=EDGE_CURVE('',#3272,#3243,#1547,.T.);
#4137=EDGE_CURVE('',#3242,#3253,#1548,.T.);
#4138=EDGE_CURVE('',#3245,#3331,#1549,.T.);
#4139=EDGE_CURVE('',#3331,#3332,#2166,.T.);
#4140=EDGE_CURVE('',#3332,#3246,#1550,.T.);
#4141=EDGE_CURVE('',#3333,#3247,#1551,.T.);
#4142=EDGE_CURVE('',#3332,#3333,#1552,.T.);
#4143=EDGE_CURVE('',#3256,#3331,#1553,.T.);
#4144=EDGE_CURVE('',#3333,#3328,#1554,.T.);
#4145=EDGE_CURVE('',#3242,#3324,#1555,.T.);
#4146=EDGE_CURVE('',#3327,#3239,#1556,.T.);
#4147=EDGE_CURVE('',#3327,#3334,#2167,.T.);
#4148=EDGE_CURVE('',#3334,#3240,#1557,.F.);
#4149=EDGE_CURVE('',#3326,#3335,#2168,.T.);
#4150=EDGE_CURVE('',#3335,#3334,#2169,.T.);
#4151=EDGE_CURVE('',#3325,#3336,#2170,.T.);
#4152=EDGE_CURVE('',#3336,#3335,#1558,.T.);
#4153=EDGE_CURVE('',#3337,#3324,#2171,.T.);
#4154=EDGE_CURVE('',#3337,#3336,#2172,.T.);
#4155=EDGE_CURVE('',#3241,#3337,#1559,.F.);
#4156=EDGE_CURVE('',#3330,#3281,#2173,.T.);
#4157=EDGE_CURVE('',#3282,#3329,#2174,.T.);
#4158=EDGE_CURVE('',#3338,#3328,#2175,.T.);
#4159=EDGE_CURVE('',#3339,#3338,#1560,.T.);
#4160=EDGE_CURVE('',#3283,#3339,#2176,.T.);
#4161=EDGE_CURVE('',#3333,#3340,#2177,.T.);
#4162=EDGE_CURVE('',#3338,#3340,#1561,.T.);
#4163=EDGE_CURVE('',#3332,#3341,#2178,.T.);
#4164=EDGE_CURVE('',#3341,#3340,#1562,.T.);
#4165=EDGE_CURVE('',#3342,#3331,#2179,.T.);
#4166=EDGE_CURVE('',#3342,#3341,#2180,.T.);
#4167=EDGE_CURVE('',#3261,#3342,#1563,.F.);
#4168=EDGE_CURVE('',#3219,#3343,#2181,.T.);
#4169=EDGE_CURVE('',#3227,#3343,#2182,.T.);
#4170=EDGE_CURVE('',#3229,#3344,#2183,.T.);
#4171=EDGE_CURVE('',#3344,#3345,#2184,.T.);
#4172=EDGE_CURVE('',#3225,#3345,#2185,.T.);
#4173=EDGE_CURVE('',#3343,#3344,#1564,.T.);
#4174=EDGE_CURVE('',#3346,#3238,#1565,.T.);
#4175=EDGE_CURVE('',#3345,#3346,#2186,.T.);
#4176=EDGE_CURVE('',#3347,#3339,#2187,.T.);
#4177=EDGE_CURVE('',#3347,#3260,#1566,.T.);
#4178=EDGE_CURVE('',#3231,#3348,#2188,.T.);
#4179=EDGE_CURVE('',#3348,#3236,#2189,.T.);
#4180=EDGE_CURVE('',#3221,#3349,#2190,.T.);
#4181=EDGE_CURVE('',#3349,#3348,#1567,.T.);
#4182=EDGE_CURVE('',#3350,#3220,#2191,.T.);
#4183=EDGE_CURVE('',#3350,#3349,#2192,.T.);
#4184=EDGE_CURVE('',#3351,#3350,#2193,.T.);
#4185=EDGE_CURVE('',#3257,#3351,#1568,.T.);
#4186=EDGE_CURVE('',#3284,#3347,#2194,.T.);
#4187=EDGE_CURVE('',#3285,#3351,#2195,.T.);
#4188=EDGE_CURVE('',#3204,#3346,#2196,.T.);
#4189=EDGE_CURVE('',#3352,#3353,#2197,.T.);
#4190=EDGE_CURVE('',#3354,#3353,#2198,.T.);
#4191=EDGE_CURVE('',#3355,#3354,#1569,.T.);
#4192=EDGE_CURVE('',#3356,#3355,#2199,.T.);
#4193=EDGE_CURVE('',#3357,#3356,#1570,.T.);
#4194=EDGE_CURVE('',#3358,#3357,#2200,.T.);
#4195=EDGE_CURVE('',#3358,#3359,#1571,.T.);
#4196=EDGE_CURVE('',#3360,#3359,#2201,.T.);
#4197=EDGE_CURVE('',#3361,#3360,#1572,.T.);
#4198=EDGE_CURVE('',#3362,#3361,#2202,.T.);
#4199=EDGE_CURVE('',#3362,#3363,#2203,.T.);
#4200=EDGE_CURVE('',#3363,#3364,#2204,.T.);
#4201=EDGE_CURVE('',#3364,#3365,#2205,.T.);
#4202=EDGE_CURVE('',#3365,#3366,#1573,.T.);
#4203=EDGE_CURVE('',#3366,#3367,#1574,.T.);
#4204=EDGE_CURVE('',#3367,#3368,#2206,.T.);
#4205=EDGE_CURVE('',#3368,#3352,#1575,.T.);
#4206=EDGE_CURVE('',#3369,#3369,#1576,.T.);
#4207=EDGE_CURVE('',#3370,#3370,#1577,.T.);
#4208=EDGE_CURVE('',#3371,#3372,#1578,.T.);
#4209=EDGE_CURVE('',#3372,#3373,#1579,.T.);
#4210=EDGE_CURVE('',#3373,#3374,#1580,.T.);
#4211=EDGE_CURVE('',#3374,#3371,#1581,.T.);
#4212=EDGE_CURVE('',#3375,#3376,#1582,.T.);
#4213=EDGE_CURVE('',#3376,#3372,#2207,.T.);
#4214=EDGE_CURVE('',#3371,#3375,#2208,.T.);
#4215=EDGE_CURVE('',#3377,#3378,#1583,.T.);
#4216=EDGE_CURVE('',#3378,#3379,#1584,.T.);
#4217=EDGE_CURVE('',#3379,#3380,#1585,.T.);
#4218=EDGE_CURVE('',#3380,#3377,#1586,.T.);
#4219=EDGE_CURVE('',#3381,#3380,#2209,.T.);
#4220=EDGE_CURVE('',#3379,#3382,#2210,.T.);
#4221=EDGE_CURVE('',#3382,#3381,#239,.T.);
#4222=EDGE_CURVE('',#3382,#3383,#2211,.T.);
#4223=EDGE_CURVE('',#3383,#3384,#1587,.T.);
#4224=EDGE_CURVE('',#3384,#3381,#2212,.T.);
#4225=EDGE_CURVE('',#3383,#3376,#1588,.T.);
#4226=EDGE_CURVE('',#3375,#3384,#1589,.T.);
#4227=EDGE_CURVE('',#3385,#3372,#2213,.T.);
#4228=EDGE_CURVE('',#3386,#3385,#1590,.T.);
#4229=EDGE_CURVE('',#3386,#3373,#2214,.T.);
#4230=EDGE_CURVE('',#3387,#3376,#2215,.T.);
#4231=EDGE_CURVE('',#3385,#3387,#2216,.T.);
#4232=EDGE_CURVE('',#3383,#3388,#2217,.T.);
#4233=EDGE_CURVE('',#3388,#3389,#2218,.T.);
#4234=EDGE_CURVE('',#3389,#3387,#1591,.F.);
#4235=EDGE_CURVE('',#3390,#3382,#2219,.T.);
#4236=EDGE_CURVE('',#3390,#3388,#2220,.T.);
#4237=EDGE_CURVE('',#3391,#3391,#1592,.F.);
#4238=EDGE_CURVE('',#3392,#3379,#2221,.T.);
#4239=EDGE_CURVE('',#3393,#3392,#2222,.T.);
#4240=EDGE_CURVE('',#3393,#3394,#2223,.T.);
#4241=EDGE_CURVE('',#3395,#3394,#2224,.T.);
#4242=EDGE_CURVE('',#3390,#3395,#2225,.T.);
#4243=EDGE_CURVE('',#3373,#3378,#2226,.T.);
#4244=EDGE_CURVE('',#3377,#3374,#2227,.T.);
#4245=EDGE_CURVE('',#3396,#3378,#2228,.T.);
#4246=EDGE_CURVE('',#3392,#3396,#1593,.T.);
#4247=EDGE_CURVE('',#3389,#3397,#2229,.T.);
#4248=EDGE_CURVE('',#3397,#3398,#2230,.T.);
#4249=EDGE_CURVE('',#3399,#3398,#2231,.T.);
#4250=EDGE_CURVE('',#3354,#3399,#2232,.T.);
#4251=EDGE_CURVE('',#3353,#3400,#2233,.T.);
#4252=EDGE_CURVE('',#3400,#3401,#1594,.T.);
#4253=EDGE_CURVE('',#3401,#3402,#2234,.T.);
#4254=EDGE_CURVE('',#3402,#3393,#1595,.T.);
#4255=EDGE_CURVE('',#3396,#3386,#2235,.T.);
#4256=EDGE_CURVE('',#3403,#3403,#1596,.T.);
#4257=EDGE_CURVE('',#3403,#3391,#2236,.T.);
#4258=EDGE_CURVE('',#3404,#3352,#2237,.T.);
#4259=EDGE_CURVE('',#3400,#3404,#2238,.T.);
#4260=EDGE_CURVE('',#3401,#3405,#2239,.T.);
#4261=EDGE_CURVE('',#3406,#3405,#2240,.T.);
#4262=EDGE_CURVE('',#3402,#3406,#2241,.T.);
#4263=EDGE_CURVE('',#3407,#3404,#1951,.T.);
#4264=EDGE_CURVE('',#3405,#3407,#1597,.T.);
#4265=EDGE_CURVE('',#3394,#3406,#1598,.T.);
#4266=EDGE_CURVE('',#3395,#3408,#2242,.T.);
#4267=EDGE_CURVE('',#3408,#3409,#1599,.T.);
#4268=EDGE_CURVE('',#3409,#3410,#2243,.T.);
#4269=EDGE_CURVE('',#3410,#3411,#1600,.T.);
#4270=EDGE_CURVE('',#3411,#3412,#2244,.T.);
#4271=EDGE_CURVE('',#3412,#3413,#2245,.T.);
#4272=EDGE_CURVE('',#3413,#3414,#2246,.T.);
#4273=EDGE_CURVE('',#3415,#3414,#2247,.T.);
#4274=EDGE_CURVE('',#3416,#3415,#1601,.T.);
#4275=EDGE_CURVE('',#3417,#3416,#2248,.T.);
#4276=EDGE_CURVE('',#3397,#3417,#1602,.T.);
#4277=EDGE_CURVE('',#3418,#3418,#1603,.T.);
#4278=EDGE_CURVE('',#3419,#3419,#1604,.T.);
#4279=EDGE_CURVE('',#3420,#3421,#1605,.T.);
#4280=EDGE_CURVE('',#3422,#3420,#2249,.T.);
#4281=EDGE_CURVE('',#3423,#3422,#1606,.T.);
#4282=EDGE_CURVE('',#3423,#3421,#2250,.T.);
#4283=EDGE_CURVE('',#3421,#3413,#2251,.T.);
#4284=EDGE_CURVE('',#3414,#3423,#2252,.T.);
#4285=EDGE_CURVE('',#3363,#3424,#2253,.T.);
#4286=EDGE_CURVE('',#3425,#3362,#2254,.T.);
#4287=EDGE_CURVE('',#3425,#3424,#2255,.T.);
#4288=EDGE_CURVE('',#3424,#3426,#1607,.T.);
#4289=EDGE_CURVE('',#3427,#3425,#1608,.T.);
#4290=EDGE_CURVE('',#3427,#3426,#2256,.T.);
#4291=EDGE_CURVE('',#3426,#3420,#2257,.T.);
#4292=EDGE_CURVE('',#3422,#3427,#2258,.T.);
#4293=EDGE_CURVE('',#3361,#3428,#2259,.T.);
#4294=EDGE_CURVE('',#3429,#3428,#2260,.T.);
#4295=EDGE_CURVE('',#3415,#3429,#2261,.T.);
#4296=EDGE_CURVE('',#3407,#3430,#2262,.T.);
#4297=EDGE_CURVE('',#3430,#3431,#2263,.T.);
#4298=EDGE_CURVE('',#3431,#3408,#2264,.T.);
#4299=EDGE_CURVE('',#3430,#3432,#1609,.T.);
#4300=EDGE_CURVE('',#3433,#3432,#2265,.F.);
#4301=EDGE_CURVE('',#3433,#3434,#1610,.T.);
#4302=EDGE_CURVE('',#3435,#3434,#1611,.F.);
#4303=EDGE_CURVE('',#3435,#3436,#2266,.T.);
#4304=EDGE_CURVE('',#3437,#3436,#2267,.T.);
#4305=EDGE_CURVE('',#3438,#3437,#2268,.T.);
#4306=EDGE_CURVE('',#3438,#3439,#1612,.T.);
#4307=EDGE_CURVE('',#3440,#3439,#2269,.T.);
#4308=EDGE_CURVE('',#3440,#3431,#1613,.T.);
#4309=EDGE_CURVE('',#3432,#3368,#2270,.T.);
#4310=EDGE_CURVE('',#3367,#3433,#2271,.T.);
#4311=EDGE_CURVE('',#3411,#3438,#2272,.T.);
#4312=EDGE_CURVE('',#3437,#3412,#2273,.T.);
#4313=EDGE_CURVE('',#3439,#3410,#2274,.T.);
#4314=EDGE_CURVE('',#3409,#3440,#2275,.T.);
#4315=EDGE_CURVE('',#3434,#3366,#2276,.T.);
#4316=EDGE_CURVE('',#3365,#3435,#2277,.T.);
#4317=EDGE_CURVE('',#3436,#3364,#2278,.T.);
#4318=EDGE_CURVE('',#3369,#3441,#2279,.T.);
#4319=EDGE_CURVE('',#3441,#3441,#1614,.T.);
#4320=EDGE_CURVE('',#3419,#3442,#2280,.T.);
#4321=EDGE_CURVE('',#3442,#3442,#1615,.T.);
#4322=EDGE_CURVE('',#3418,#3443,#2281,.T.);
#4323=EDGE_CURVE('',#3443,#3443,#1616,.T.);
#4324=EDGE_CURVE('',#3370,#3444,#2282,.T.);
#4325=EDGE_CURVE('',#3444,#3444,#1617,.T.);
#4326=EDGE_CURVE('',#3445,#3446,#1618,.T.);
#4327=EDGE_CURVE('',#3446,#3447,#2283,.T.);
#4328=EDGE_CURVE('',#3447,#3448,#1619,.T.);
#4329=EDGE_CURVE('',#3448,#3445,#2284,.T.);
#4330=EDGE_CURVE('',#3449,#3450,#1620,.T.);
#4331=EDGE_CURVE('',#3450,#3448,#1621,.T.);
#4332=EDGE_CURVE('',#3447,#3449,#1622,.T.);
#4333=EDGE_CURVE('',#3451,#3452,#1623,.T.);
#4334=EDGE_CURVE('',#3452,#3450,#2285,.T.);
#4335=EDGE_CURVE('',#3449,#3451,#2286,.T.);
#4336=EDGE_CURVE('',#3453,#3454,#1624,.T.);
#4337=EDGE_CURVE('',#3454,#3452,#1625,.T.);
#4338=EDGE_CURVE('',#3451,#3453,#1626,.T.);
#4339=EDGE_CURVE('',#3455,#3456,#1627,.T.);
#4340=EDGE_CURVE('',#3456,#3454,#2287,.T.);
#4341=EDGE_CURVE('',#3453,#3455,#2288,.T.);
#4342=EDGE_CURVE('',#3399,#3457,#1628,.T.);
#4343=EDGE_CURVE('',#3457,#3456,#1629,.T.);
#4344=EDGE_CURVE('',#3455,#3399,#1630,.T.);
#4345=EDGE_CURVE('',#3398,#3458,#1631,.T.);
#4346=EDGE_CURVE('',#3458,#3457,#2289,.T.);
#4347=EDGE_CURVE('',#3459,#3460,#1632,.T.);
#4348=EDGE_CURVE('',#3460,#3458,#1633,.T.);
#4349=EDGE_CURVE('',#3398,#3459,#1634,.T.);
#4350=EDGE_CURVE('',#3461,#3462,#1635,.T.);
#4351=EDGE_CURVE('',#3462,#3460,#2290,.T.);
#4352=EDGE_CURVE('',#3459,#3461,#2291,.T.);
#4353=EDGE_CURVE('',#3429,#3463,#1636,.T.);
#4354=EDGE_CURVE('',#3463,#3462,#1637,.T.);
#4355=EDGE_CURVE('',#3461,#3429,#1638,.T.);
#4356=EDGE_CURVE('',#3428,#3464,#1639,.T.);
#4357=EDGE_CURVE('',#3464,#3463,#2292,.T.);
#4358=EDGE_CURVE('',#3445,#3464,#1640,.T.);
#4359=EDGE_CURVE('',#3428,#3446,#1641,.T.);
#4360=EDGE_CURVE('',#3355,#3455,#2293,.T.);
#4361=EDGE_CURVE('',#3356,#3453,#2294,.T.);
#4362=EDGE_CURVE('',#3357,#3451,#2295,.T.);
#4363=EDGE_CURVE('',#3358,#3449,#2296,.T.);
#4364=EDGE_CURVE('',#3359,#3447,#2297,.T.);
#4365=EDGE_CURVE('',#3360,#3446,#2298,.T.);
#4366=EDGE_CURVE('',#3416,#3461,#2299,.T.);
#4367=EDGE_CURVE('',#3417,#3459,#2300,.T.);
#4368=EDGE_CURVE('',#3465,#3465,#1642,.T.);
#4369=EDGE_CURVE('',#3465,#3466,#2301,.T.);
#4370=EDGE_CURVE('',#3466,#3466,#1643,.T.);
#4371=EDGE_CURVE('',#3467,#3467,#1644,.T.);
#4372=EDGE_CURVE('',#3467,#3468,#2302,.T.);
#4373=EDGE_CURVE('',#3468,#3468,#1645,.T.);
#4374=EDGE_CURVE('',#3469,#3469,#1646,.T.);
#4375=EDGE_CURVE('',#3469,#3470,#2303,.T.);
#4376=EDGE_CURVE('',#3470,#3470,#1647,.T.);
#4377=EDGE_CURVE('',#3471,#3471,#1648,.T.);
#4378=EDGE_CURVE('',#3471,#3472,#2304,.T.);
#4379=EDGE_CURVE('',#3472,#3472,#1649,.T.);
#4380=EDGE_CURVE('',#3473,#3474,#1650,.T.);
#4381=EDGE_CURVE('',#3474,#3475,#2305,.T.);
#4382=EDGE_CURVE('',#3475,#3476,#1651,.T.);
#4383=EDGE_CURVE('',#3476,#3477,#2306,.T.);
#4384=EDGE_CURVE('',#3477,#3478,#1652,.T.);
#4385=EDGE_CURVE('',#3478,#3479,#2307,.T.);
#4386=EDGE_CURVE('',#3479,#3480,#1653,.T.);
#4387=EDGE_CURVE('',#3480,#3473,#2308,.T.);
#4388=EDGE_CURVE('',#3481,#3482,#1654,.T.);
#4389=EDGE_CURVE('',#3482,#3483,#2309,.T.);
#4390=EDGE_CURVE('',#3483,#3484,#1655,.T.);
#4391=EDGE_CURVE('',#3484,#3485,#2310,.T.);
#4392=EDGE_CURVE('',#3485,#3486,#1656,.T.);
#4393=EDGE_CURVE('',#3486,#3487,#2311,.T.);
#4394=EDGE_CURVE('',#3487,#3488,#1657,.T.);
#4395=EDGE_CURVE('',#3488,#3481,#2312,.T.);
#4396=EDGE_CURVE('',#3489,#3482,#2313,.T.);
#4397=EDGE_CURVE('',#3490,#3489,#2314,.T.);
#4398=EDGE_CURVE('',#3483,#3490,#2315,.T.);
#4399=EDGE_CURVE('',#3491,#3490,#1658,.T.);
#4400=EDGE_CURVE('',#3484,#3491,#2316,.T.);
#4401=EDGE_CURVE('',#3492,#3491,#2317,.T.);
#4402=EDGE_CURVE('',#3485,#3492,#2318,.T.);
#4403=EDGE_CURVE('',#3493,#3492,#1659,.T.);
#4404=EDGE_CURVE('',#3486,#3493,#2319,.T.);
#4405=EDGE_CURVE('',#3494,#3493,#2320,.T.);
#4406=EDGE_CURVE('',#3487,#3494,#2321,.T.);
#4407=EDGE_CURVE('',#3495,#3494,#1660,.T.);
#4408=EDGE_CURVE('',#3488,#3495,#2322,.T.);
#4409=EDGE_CURVE('',#3496,#3495,#2323,.T.);
#4410=EDGE_CURVE('',#3481,#3496,#2324,.T.);
#4411=EDGE_CURVE('',#3489,#3496,#1661,.T.);
#4412=EDGE_CURVE('',#3497,#3474,#2325,.T.);
#4413=EDGE_CURVE('',#3498,#3497,#2326,.T.);
#4414=EDGE_CURVE('',#3475,#3498,#2327,.T.);
#4415=EDGE_CURVE('',#3499,#3498,#1662,.T.);
#4416=EDGE_CURVE('',#3476,#3499,#2328,.T.);
#4417=EDGE_CURVE('',#3500,#3499,#2329,.T.);
#4418=EDGE_CURVE('',#3477,#3500,#2330,.T.);
#4419=EDGE_CURVE('',#3501,#3500,#1663,.T.);
#4420=EDGE_CURVE('',#3478,#3501,#2331,.T.);
#4421=EDGE_CURVE('',#3502,#3501,#2332,.T.);
#4422=EDGE_CURVE('',#3479,#3502,#2333,.T.);
#4423=EDGE_CURVE('',#3503,#3502,#1664,.T.);
#4424=EDGE_CURVE('',#3480,#3503,#2334,.T.);
#4425=EDGE_CURVE('',#3504,#3503,#2335,.T.);
#4426=EDGE_CURVE('',#3473,#3504,#2336,.T.);
#4427=EDGE_CURVE('',#3497,#3504,#1665,.T.);
#4428=EDGE_CURVE('',#3505,#3506,#1666,.T.);
#4429=EDGE_CURVE('',#3506,#3507,#2337,.T.);
#4430=EDGE_CURVE('',#3507,#3508,#1667,.T.);
#4431=EDGE_CURVE('',#3508,#3505,#2338,.T.);
#4432=EDGE_CURVE('',#3508,#3509,#1668,.T.);
#4433=EDGE_CURVE('',#3509,#3510,#2339,.T.);
#4434=EDGE_CURVE('',#3510,#3511,#1669,.T.);
#4435=EDGE_CURVE('',#3511,#3508,#2340,.T.);
#4436=EDGE_CURVE('',#3507,#3509,#1670,.T.);
#4437=EDGE_CURVE('',#3511,#3512,#1671,.T.);
#4438=EDGE_CURVE('',#3512,#3513,#2341,.T.);
#4439=EDGE_CURVE('',#3513,#3514,#1672,.T.);
#4440=EDGE_CURVE('',#3514,#3511,#2342,.T.);
#4441=EDGE_CURVE('',#3510,#3512,#1673,.T.);
#4442=EDGE_CURVE('',#3514,#3515,#1674,.T.);
#4443=EDGE_CURVE('',#3515,#3516,#2343,.T.);
#4444=EDGE_CURVE('',#3516,#3505,#1675,.T.);
#4445=EDGE_CURVE('',#3505,#3514,#2344,.T.);
#4446=EDGE_CURVE('',#3513,#3515,#1676,.T.);
#4447=EDGE_CURVE('',#3516,#3506,#1677,.T.);
#4448=EDGE_CURVE('',#3517,#3507,#2345,.T.);
#4449=EDGE_CURVE('',#3517,#3518,#1678,.T.);
#4450=EDGE_CURVE('',#3518,#3509,#2346,.T.);
#4451=EDGE_CURVE('',#3519,#3506,#2347,.T.);
#4452=EDGE_CURVE('',#3519,#3517,#2348,.T.);
#4453=EDGE_CURVE('',#3520,#3516,#2349,.T.);
#4454=EDGE_CURVE('',#3520,#3519,#1679,.T.);
#4455=EDGE_CURVE('',#3521,#3515,#2350,.T.);
#4456=EDGE_CURVE('',#3521,#3520,#2351,.T.);
#4457=EDGE_CURVE('',#3522,#3522,#1680,.T.);
#4458=EDGE_CURVE('',#3523,#3524,#1681,.T.);
#4459=EDGE_CURVE('',#3524,#3525,#1682,.T.);
#4460=EDGE_CURVE('',#3525,#3523,#1683,.T.);
#4461=EDGE_CURVE('',#3526,#3527,#1684,.T.);
#4462=EDGE_CURVE('',#3527,#3524,#2352,.T.);
#4463=EDGE_CURVE('',#3523,#3526,#2353,.T.);
#4464=EDGE_CURVE('',#3528,#3529,#1685,.T.);
#4465=EDGE_CURVE('',#3529,#3527,#1952,.T.);
#4466=EDGE_CURVE('',#3526,#3528,#1953,.T.);
#4467=EDGE_CURVE('',#3530,#3531,#1686,.T.);
#4468=EDGE_CURVE('',#3531,#3529,#240,.T.);
#4469=EDGE_CURVE('',#3528,#3530,#241,.T.);
#4470=EDGE_CURVE('',#3532,#3533,#1687,.T.);
#4471=EDGE_CURVE('',#3533,#3531,#1954,.T.);
#4472=EDGE_CURVE('',#3530,#3532,#1955,.T.);
#4473=EDGE_CURVE('',#3534,#3535,#1688,.T.);
#4474=EDGE_CURVE('',#3535,#3533,#2354,.T.);
#4475=EDGE_CURVE('',#3532,#3534,#2355,.T.);
#4476=EDGE_CURVE('',#3534,#3536,#1689,.T.);
#4477=EDGE_CURVE('',#3536,#3535,#1690,.T.);
#4478=EDGE_CURVE('',#3532,#3537,#2356,.T.);
#4479=EDGE_CURVE('',#3538,#3537,#2357,.T.);
#4480=EDGE_CURVE('',#3534,#3538,#2358,.T.);
#4481=EDGE_CURVE('',#3539,#3530,#2359,.T.);
#4482=EDGE_CURVE('',#3537,#3539,#1691,.T.);
#4483=EDGE_CURVE('',#3528,#3540,#2360,.T.);
#4484=EDGE_CURVE('',#3541,#3540,#2361,.T.);
#4485=EDGE_CURVE('',#3541,#3542,#2362,.T.);
#4486=EDGE_CURVE('',#3539,#3542,#2363,.T.);
#4487=EDGE_CURVE('',#3543,#3526,#2364,.T.);
#4488=EDGE_CURVE('',#3540,#3543,#1692,.T.);
#4489=EDGE_CURVE('',#3544,#3523,#2365,.T.);
#4490=EDGE_CURVE('',#3543,#3544,#2366,.T.);
#4491=EDGE_CURVE('',#3525,#3545,#2367,.T.);
#4492=EDGE_CURVE('',#3544,#3545,#1693,.T.);
#4493=EDGE_CURVE('',#3524,#3546,#1694,.T.);
#4494=EDGE_CURVE('',#3546,#3547,#1695,.T.);
#4495=EDGE_CURVE('',#3548,#3547,#1696,.T.);
#4496=EDGE_CURVE('',#3548,#3525,#1697,.T.);
#4497=EDGE_CURVE('',#3549,#3550,#1698,.T.);
#4498=EDGE_CURVE('',#3550,#3551,#1699,.T.);
#4499=EDGE_CURVE('',#3551,#3549,#1700,.T.);
#4500=EDGE_CURVE('',#3552,#3553,#1701,.T.);
#4501=EDGE_CURVE('',#3553,#3550,#2368,.T.);
#4502=EDGE_CURVE('',#3549,#3552,#2369,.T.);
#4503=EDGE_CURVE('',#3554,#3555,#1702,.T.);
#4504=EDGE_CURVE('',#3555,#3553,#1956,.T.);
#4505=EDGE_CURVE('',#3552,#3554,#1957,.T.);
#4506=EDGE_CURVE('',#3556,#3557,#1703,.T.);
#4507=EDGE_CURVE('',#3557,#3555,#242,.T.);
#4508=EDGE_CURVE('',#3554,#3556,#243,.T.);
#4509=EDGE_CURVE('',#3558,#3559,#1704,.T.);
#4510=EDGE_CURVE('',#3559,#3557,#1958,.T.);
#4511=EDGE_CURVE('',#3556,#3558,#1959,.T.);
#4512=EDGE_CURVE('',#3560,#3547,#1705,.T.);
#4513=EDGE_CURVE('',#3547,#3559,#2370,.T.);
#4514=EDGE_CURVE('',#3558,#3560,#2371,.T.);
#4515=EDGE_CURVE('',#3560,#3548,#1706,.T.);
#4516=EDGE_CURVE('',#3561,#3558,#2372,.T.);
#4517=EDGE_CURVE('',#3562,#3561,#2373,.T.);
#4518=EDGE_CURVE('',#3560,#3562,#2374,.T.);
#4519=EDGE_CURVE('',#3563,#3556,#2375,.T.);
#4520=EDGE_CURVE('',#3561,#3563,#1707,.T.);
#4521=EDGE_CURVE('',#3554,#3564,#2376,.T.);
#4522=EDGE_CURVE('',#3565,#3564,#2377,.T.);
#4523=EDGE_CURVE('',#3566,#3565,#2378,.T.);
#4524=EDGE_CURVE('',#3563,#3566,#2379,.T.);
#4525=EDGE_CURVE('',#3552,#3567,#2380,.T.);
#4526=EDGE_CURVE('',#3564,#3567,#1708,.T.);
#4527=EDGE_CURVE('',#3568,#3549,#2381,.T.);
#4528=EDGE_CURVE('',#3567,#3568,#2382,.T.);
#4529=EDGE_CURVE('',#3551,#3569,#2383,.T.);
#4530=EDGE_CURVE('',#3568,#3569,#1709,.T.);
#4531=EDGE_CURVE('',#3536,#3551,#1710,.T.);
#4532=EDGE_CURVE('',#3550,#3535,#1711,.T.);
#4533=EDGE_CURVE('',#3538,#3570,#1712,.T.);
#4534=EDGE_CURVE('',#3570,#3536,#2384,.T.);
#4535=EDGE_CURVE('',#3571,#3572,#1713,.T.);
#4536=EDGE_CURVE('',#3572,#3570,#1714,.T.);
#4537=EDGE_CURVE('',#3538,#3571,#1715,.T.);
#4538=EDGE_CURVE('',#3573,#3574,#1716,.T.);
#4539=EDGE_CURVE('',#3574,#3572,#2385,.T.);
#4540=EDGE_CURVE('',#3571,#3573,#2386,.T.);
#4541=EDGE_CURVE('',#3569,#3574,#1717,.T.);
#4542=EDGE_CURVE('',#3573,#3568,#1718,.T.);
#4543=EDGE_CURVE('',#3537,#3575,#1719,.T.);
#4544=EDGE_CURVE('',#3575,#3571,#2387,.T.);
#4545=EDGE_CURVE('',#3522,#3546,#2388,.T.);
#4546=EDGE_CURVE('',#3562,#3576,#1720,.T.);
#4547=EDGE_CURVE('',#3576,#3548,#2389,.T.);
#4548=EDGE_CURVE('',#3577,#3578,#1721,.T.);
#4549=EDGE_CURVE('',#3578,#3576,#1722,.T.);
#4550=EDGE_CURVE('',#3562,#3577,#1723,.T.);
#4551=EDGE_CURVE('',#3579,#3580,#1724,.T.);
#4552=EDGE_CURVE('',#3580,#3578,#2390,.T.);
#4553=EDGE_CURVE('',#3577,#3579,#2391,.T.);
#4554=EDGE_CURVE('',#3545,#3580,#1725,.T.);
#4555=EDGE_CURVE('',#3579,#3544,#1726,.T.);
#4556=EDGE_CURVE('',#3561,#3581,#1727,.T.);
#4557=EDGE_CURVE('',#3581,#3577,#2392,.T.);
#4558=EDGE_CURVE('',#3582,#3565,#1728,.T.);
#4559=EDGE_CURVE('',#3564,#3583,#1729,.T.);
#4560=EDGE_CURVE('',#3583,#3582,#2393,.T.);
#4561=EDGE_CURVE('',#3567,#3584,#1730,.T.);
#4562=EDGE_CURVE('',#3584,#3583,#1731,.T.);
#4563=EDGE_CURVE('',#3573,#3584,#2394,.T.);
#4564=EDGE_CURVE('',#3585,#3586,#1732,.T.);
#4565=EDGE_CURVE('',#3586,#3565,#1733,.T.);
#4566=EDGE_CURVE('',#3582,#3585,#1734,.T.);
#4567=EDGE_CURVE('',#3587,#3575,#1735,.T.);
#4568=EDGE_CURVE('',#3588,#3587,#2395,.T.);
#4569=EDGE_CURVE('',#3589,#3588,#1736,.T.);
#4570=EDGE_CURVE('',#3590,#3589,#2396,.T.);
#4571=EDGE_CURVE('',#3591,#3590,#2397,.T.);
#4572=EDGE_CURVE('',#3591,#3585,#2398,.T.);
#4573=EDGE_CURVE('',#3592,#3593,#1737,.T.);
#4574=EDGE_CURVE('',#3593,#3592,#2399,.T.);
#4575=EDGE_CURVE('',#3539,#3587,#1738,.T.);
#4576=EDGE_CURVE('',#3542,#3588,#1739,.T.);
#4577=EDGE_CURVE('',#3594,#3589,#1740,.T.);
#4578=EDGE_CURVE('',#3542,#3594,#1741,.T.);
#4579=EDGE_CURVE('',#3595,#3541,#1742,.T.);
#4580=EDGE_CURVE('',#3540,#3596,#1743,.T.);
#4581=EDGE_CURVE('',#3596,#3595,#2400,.T.);
#4582=EDGE_CURVE('',#3543,#3597,#1744,.T.);
#4583=EDGE_CURVE('',#3597,#3596,#1745,.T.);
#4584=EDGE_CURVE('',#3579,#3597,#2401,.T.);
#4585=EDGE_CURVE('',#3598,#3599,#1746,.T.);
#4586=EDGE_CURVE('',#3599,#3541,#1747,.T.);
#4587=EDGE_CURVE('',#3595,#3598,#1748,.T.);
#4588=EDGE_CURVE('',#3600,#3581,#1749,.T.);
#4589=EDGE_CURVE('',#3601,#3600,#2402,.T.);
#4590=EDGE_CURVE('',#3602,#3601,#1750,.T.);
#4591=EDGE_CURVE('',#3603,#3602,#2403,.T.);
#4592=EDGE_CURVE('',#3604,#3603,#2404,.T.);
#4593=EDGE_CURVE('',#3604,#3598,#2405,.T.);
#4594=EDGE_CURVE('',#3605,#3606,#2406,.T.);
#4595=EDGE_CURVE('',#3606,#3605,#1751,.T.);
#4596=EDGE_CURVE('',#3563,#3600,#1752,.T.);
#4597=EDGE_CURVE('',#3566,#3601,#1753,.T.);
#4598=EDGE_CURVE('',#3607,#3602,#1754,.T.);
#4599=EDGE_CURVE('',#3566,#3607,#1755,.T.);
#4600=EDGE_CURVE('',#3594,#3599,#2407,.T.);
#4601=EDGE_CURVE('',#3586,#3607,#2408,.T.);
#4602=EDGE_CURVE('',#3608,#3599,#2409,.T.);
#4603=EDGE_CURVE('',#3609,#3608,#2410,.T.);
#4604=EDGE_CURVE('',#3609,#3594,#2411,.T.);
#4605=EDGE_CURVE('',#3610,#3586,#2412,.T.);
#4606=EDGE_CURVE('',#3611,#3610,#2413,.T.);
#4607=EDGE_CURVE('',#3611,#3607,#2414,.T.);
#4608=EDGE_CURVE('',#3592,#3612,#2415,.T.);
#4609=EDGE_CURVE('',#3613,#3612,#1756,.T.);
#4610=EDGE_CURVE('',#3613,#3593,#2416,.T.);
#4611=EDGE_CURVE('',#3612,#3613,#2417,.T.);
#4612=EDGE_CURVE('',#3614,#3605,#2418,.T.);
#4613=EDGE_CURVE('',#3615,#3614,#2419,.T.);
#4614=EDGE_CURVE('',#3606,#3615,#2420,.T.);
#4615=EDGE_CURVE('',#3614,#3615,#1757,.T.);
#4616=EDGE_CURVE('',#3608,#3604,#1758,.T.);
#4617=EDGE_CURVE('',#3603,#3611,#1759,.T.);
#4618=EDGE_CURVE('',#3610,#3591,#1760,.T.);
#4619=EDGE_CURVE('',#3590,#3609,#1761,.T.);
#4620=EDGE_CURVE('',#3616,#3513,#2421,.T.);
#4621=EDGE_CURVE('',#3616,#3521,#1762,.T.);
#4622=EDGE_CURVE('',#3617,#3512,#2422,.T.);
#4623=EDGE_CURVE('',#3617,#3616,#2423,.T.);
#4624=EDGE_CURVE('',#3618,#3510,#2424,.T.);
#4625=EDGE_CURVE('',#3618,#3617,#1763,.T.);
#4626=EDGE_CURVE('',#3518,#3618,#2425,.T.);
#4627=EDGE_CURVE('',#3619,#3619,#1764,.T.);
#4628=EDGE_CURVE('',#3619,#3620,#2426,.T.);
#4629=EDGE_CURVE('',#3620,#3620,#1765,.T.);
#4630=EDGE_CURVE('',#3621,#3621,#1766,.T.);
#4631=EDGE_CURVE('',#3621,#3620,#2427,.T.);
#4632=EDGE_CURVE('',#3622,#3622,#1767,.T.);
#4633=EDGE_CURVE('',#3623,#3623,#1768,.T.);
#4634=EDGE_CURVE('',#3623,#3621,#2428,.T.);
#4635=EDGE_CURVE('',#3624,#3624,#1769,.T.);
#4636=EDGE_CURVE('',#3624,#3622,#2429,.T.);
#4637=EDGE_CURVE('',#3625,#3626,#1960,.F.);
#4638=EDGE_CURVE('',#3627,#3625,#1770,.T.);
#4639=EDGE_CURVE('',#3627,#3628,#1961,.T.);
#4640=EDGE_CURVE('',#3626,#3628,#1771,.T.);
#4641=EDGE_CURVE('',#3629,#3630,#1962,.T.);
#4642=EDGE_CURVE('',#3631,#3630,#1772,.T.);
#4643=EDGE_CURVE('',#3632,#3631,#1963,.F.);
#4644=EDGE_CURVE('',#3629,#3632,#1773,.T.);
#4645=EDGE_CURVE('',#3633,#3634,#1774,.T.);
#4646=EDGE_CURVE('',#3634,#3627,#2430,.T.);
#4647=EDGE_CURVE('',#3625,#3633,#2431,.T.);
#4648=EDGE_CURVE('',#3635,#3636,#1775,.T.);
#4649=EDGE_CURVE('',#3636,#3634,#1964,.T.);
#4650=EDGE_CURVE('',#3633,#3635,#1965,.T.);
#4651=EDGE_CURVE('',#3637,#3638,#1776,.T.);
#4652=EDGE_CURVE('',#3638,#3636,#2432,.T.);
#4653=EDGE_CURVE('',#3635,#3637,#2433,.T.);
#4654=EDGE_CURVE('',#3639,#3640,#1777,.T.);
#4655=EDGE_CURVE('',#3640,#3638,#1966,.T.);
#4656=EDGE_CURVE('',#3637,#3639,#1967,.T.);
#4657=EDGE_CURVE('',#3630,#3640,#2434,.T.);
#4658=EDGE_CURVE('',#3639,#3631,#2435,.T.);
#4659=EDGE_CURVE('',#3631,#3625,#2436,.T.);
#4660=EDGE_CURVE('',#3626,#3632,#2437,.T.);
#4661=EDGE_CURVE('',#3628,#3641,#1778,.T.);
#4662=EDGE_CURVE('',#3641,#3629,#1779,.T.);
#4663=EDGE_CURVE('',#3632,#3626,#1780,.T.);
#4664=EDGE_CURVE('',#3642,#3638,#1781,.T.);
#4665=EDGE_CURVE('',#3643,#3642,#2438,.T.);
#4666=EDGE_CURVE('',#3636,#3643,#1782,.T.);
#4667=EDGE_CURVE('',#3640,#3644,#1783,.T.);
#4668=EDGE_CURVE('',#3642,#3644,#1968,.T.);
#4669=EDGE_CURVE('',#3645,#3645,#1784,.T.);
#4670=EDGE_CURVE('',#3646,#3647,#1969,.T.);
#4671=EDGE_CURVE('',#3648,#3647,#1785,.T.);
#4672=EDGE_CURVE('',#3649,#3648,#1970,.F.);
#4673=EDGE_CURVE('',#3646,#3649,#1786,.T.);
#4674=EDGE_CURVE('',#3650,#3651,#1971,.F.);
#4675=EDGE_CURVE('',#3652,#3650,#1787,.T.);
#4676=EDGE_CURVE('',#3652,#3653,#1972,.T.);
#4677=EDGE_CURVE('',#3651,#3653,#1788,.T.);
#4678=EDGE_CURVE('',#3654,#3644,#1789,.T.);
#4679=EDGE_CURVE('',#3644,#3652,#2439,.T.);
#4680=EDGE_CURVE('',#3650,#3654,#2440,.T.);
#4681=EDGE_CURVE('',#3655,#3642,#1790,.T.);
#4682=EDGE_CURVE('',#3654,#3655,#1973,.T.);
#4683=EDGE_CURVE('',#3656,#3643,#1791,.T.);
#4684=EDGE_CURVE('',#3655,#3656,#2441,.T.);
#4685=EDGE_CURVE('',#3657,#3658,#1792,.T.);
#4686=EDGE_CURVE('',#3658,#3643,#1974,.T.);
#4687=EDGE_CURVE('',#3656,#3657,#1975,.T.);
#4688=EDGE_CURVE('',#3647,#3658,#2442,.T.);
#4689=EDGE_CURVE('',#3657,#3648,#2443,.T.);
#4690=EDGE_CURVE('',#3653,#3646,#1793,.T.);
#4691=EDGE_CURVE('',#3649,#3651,#1794,.T.);
#4692=EDGE_CURVE('',#3648,#3650,#2444,.T.);
#4693=EDGE_CURVE('',#3651,#3649,#2445,.T.);
#4694=EDGE_CURVE('',#3658,#3634,#1795,.T.);
#4695=EDGE_CURVE('',#3641,#3659,#2446,.T.);
#4696=EDGE_CURVE('',#3659,#3659,#1796,.T.);
#4697=EDGE_CURVE('',#3660,#3660,#1797,.T.);
#4698=EDGE_CURVE('',#3659,#3661,#1798,.T.);
#4699=EDGE_CURVE('',#3661,#3661,#1799,.T.);
#4700=EDGE_CURVE('',#3662,#3662,#1800,.T.);
#4701=EDGE_CURVE('',#3663,#3663,#1801,.T.);
#4702=EDGE_CURVE('',#3663,#3662,#1802,.T.);
#4703=EDGE_CURVE('',#3664,#3665,#1803,.T.);
#4704=EDGE_CURVE('',#3664,#3663,#2447,.T.);
#4705=EDGE_CURVE('',#3665,#3664,#1804,.T.);
#4706=EDGE_CURVE('',#3666,#3666,#1805,.T.);
#4707=EDGE_CURVE('',#3666,#3665,#1806,.T.);
#4708=EDGE_CURVE('',#3667,#3667,#1807,.T.);
#4709=EDGE_CURVE('',#3667,#3668,#2448,.T.);
#4710=EDGE_CURVE('',#3668,#3668,#1808,.T.);
#4711=EDGE_CURVE('',#3668,#3669,#2449,.T.);
#4712=EDGE_CURVE('',#3669,#3669,#1809,.T.);
#4713=EDGE_CURVE('',#3645,#3660,#2450,.T.);
#4714=EDGE_CURVE('',#3670,#3671,#2451,.T.);
#4715=EDGE_CURVE('',#3670,#3672,#1976,.T.);
#4716=EDGE_CURVE('',#3672,#3673,#1810,.T.);
#4717=EDGE_CURVE('',#3673,#3671,#1977,.T.);
#4718=EDGE_CURVE('',#3674,#3675,#2452,.T.);
#4719=EDGE_CURVE('',#3674,#3670,#1978,.T.);
#4720=EDGE_CURVE('',#3671,#3675,#1979,.T.);
#4721=EDGE_CURVE('',#3676,#3677,#2453,.T.);
#4722=EDGE_CURVE('',#3676,#3674,#1980,.T.);
#4723=EDGE_CURVE('',#3675,#3677,#1981,.T.);
#4724=EDGE_CURVE('',#3678,#3679,#2454,.T.);
#4725=EDGE_CURVE('',#3678,#3676,#1982,.T.);
#4726=EDGE_CURVE('',#3677,#3679,#1983,.T.);
#4727=EDGE_CURVE('',#3680,#3681,#2455,.T.);
#4728=EDGE_CURVE('',#3680,#3678,#1984,.T.);
#4729=EDGE_CURVE('',#3679,#3681,#1985,.T.);
#4730=EDGE_CURVE('',#3682,#3683,#2456,.T.);
#4731=EDGE_CURVE('',#3682,#3680,#1986,.T.);
#4732=EDGE_CURVE('',#3681,#3683,#1987,.T.);
#4733=EDGE_CURVE('',#3684,#3685,#2457,.T.);
#4734=EDGE_CURVE('',#3684,#3686,#1988,.T.);
#4735=EDGE_CURVE('',#3687,#3686,#1811,.T.);
#4736=EDGE_CURVE('',#3685,#3687,#1989,.T.);
#4737=EDGE_CURVE('',#3688,#3689,#2458,.T.);
#4738=EDGE_CURVE('',#3688,#3684,#1990,.T.);
#4739=EDGE_CURVE('',#3689,#3685,#1991,.T.);
#4740=EDGE_CURVE('',#3690,#3691,#2459,.T.);
#4741=EDGE_CURVE('',#3690,#3688,#1992,.T.);
#4742=EDGE_CURVE('',#3691,#3689,#1993,.T.);
#4743=EDGE_CURVE('',#3692,#3693,#2460,.T.);
#4744=EDGE_CURVE('',#3692,#3690,#1994,.T.);
#4745=EDGE_CURVE('',#3693,#3691,#1995,.T.);
#4746=EDGE_CURVE('',#3694,#3695,#2461,.T.);
#4747=EDGE_CURVE('',#3694,#3692,#1996,.T.);
#4748=EDGE_CURVE('',#3695,#3693,#1997,.T.);
#4749=EDGE_CURVE('',#3696,#3687,#1998,.T.);
#4750=EDGE_CURVE('',#3683,#3696,#1999,.T.);
#4751=EDGE_CURVE('',#3697,#3673,#2000,.T.);
#4752=EDGE_CURVE('',#3697,#3695,#2001,.T.);
#4753=EDGE_CURVE('',#3698,#3697,#1812,.T.);
#4754=EDGE_CURVE('',#3698,#3694,#2002,.T.);
#4755=EDGE_CURVE('',#3686,#3699,#2003,.T.);
#4756=EDGE_CURVE('',#3672,#3698,#2004,.T.);
#4757=EDGE_CURVE('',#3699,#3682,#2005,.T.);
#4758=EDGE_CURVE('',#3700,#3700,#1813,.T.);
#4759=EDGE_CURVE('',#3699,#3696,#1814,.T.);
#4760=EDGE_CURVE('',#3701,#3701,#1815,.T.);
#4761=EDGE_CURVE('',#3701,#3700,#2462,.T.);
#4762=EDGE_CURVE('',#3702,#3702,#1816,.T.);
#4763=EDGE_CURVE('',#3703,#3703,#1817,.T.);
#4764=EDGE_CURVE('',#3702,#3703,#2463,.T.);
#4765=EDGE_CURVE('',#3704,#3705,#244,.T.);
#4766=EDGE_CURVE('',#3705,#3706,#245,.T.);
#4767=EDGE_CURVE('',#3706,#3704,#1818,.T.);
#4768=EDGE_CURVE('',#3707,#3708,#246,.T.);
#4769=EDGE_CURVE('',#3708,#3709,#247,.T.);
#4770=EDGE_CURVE('',#3709,#3707,#1819,.T.);
#4771=EDGE_CURVE('',#3710,#3711,#248,.T.);
#4772=EDGE_CURVE('',#3711,#3712,#249,.T.);
#4773=EDGE_CURVE('',#3712,#3710,#1820,.T.);
#4774=EDGE_CURVE('',#3713,#3714,#250,.T.);
#4775=EDGE_CURVE('',#3714,#3715,#251,.T.);
#4776=EDGE_CURVE('',#3715,#3713,#1821,.T.);
#4777=EDGE_CURVE('',#3704,#3715,#2464,.T.);
#4778=EDGE_CURVE('',#3714,#3705,#2465,.T.);
#4779=EDGE_CURVE('',#3711,#3714,#2466,.T.);
#4780=EDGE_CURVE('',#3713,#3712,#2467,.T.);
#4781=EDGE_CURVE('',#3708,#3711,#2468,.T.);
#4782=EDGE_CURVE('',#3710,#3709,#2469,.T.);
#4783=EDGE_CURVE('',#3705,#3708,#2470,.T.);
#4784=EDGE_CURVE('',#3707,#3706,#2471,.T.);
#4785=EDGE_CURVE('',#3716,#3710,#2472,.T.);
#4786=EDGE_CURVE('',#3716,#3717,#2473,.T.);
#4787=EDGE_CURVE('',#3717,#3709,#2474,.T.);
#4788=EDGE_CURVE('',#3718,#3712,#2475,.T.);
#4789=EDGE_CURVE('',#3718,#3716,#1822,.T.);
#4790=EDGE_CURVE('',#3719,#3713,#2476,.T.);
#4791=EDGE_CURVE('',#3719,#3718,#2477,.T.);
#4792=EDGE_CURVE('',#3720,#3715,#2478,.T.);
#4793=EDGE_CURVE('',#3720,#3719,#1823,.T.);
#4794=EDGE_CURVE('',#3721,#3722,#1824,.T.);
#4795=EDGE_CURVE('',#3722,#3723,#1825,.T.);
#4796=EDGE_CURVE('',#3723,#3724,#1826,.T.);
#4797=EDGE_CURVE('',#3724,#3721,#1827,.T.);
#4798=EDGE_CURVE('',#3725,#3726,#2479,.T.);
#4799=EDGE_CURVE('',#3726,#3727,#2480,.T.);
#4800=EDGE_CURVE('',#3728,#3727,#2481,.T.);
#4801=EDGE_CURVE('',#3725,#3728,#2482,.T.);
#4802=EDGE_CURVE('',#3726,#3729,#1828,.T.);
#4803=EDGE_CURVE('',#3729,#3730,#2483,.T.);
#4804=EDGE_CURVE('',#3727,#3730,#1829,.T.);
#4805=EDGE_CURVE('',#3729,#3731,#2484,.T.);
#4806=EDGE_CURVE('',#3731,#3732,#2485,.T.);
#4807=EDGE_CURVE('',#3730,#3732,#2486,.T.);
#4808=EDGE_CURVE('',#3731,#3733,#1830,.T.);
#4809=EDGE_CURVE('',#3733,#3734,#2487,.T.);
#4810=EDGE_CURVE('',#3732,#3734,#1831,.T.);
#4811=EDGE_CURVE('',#3735,#3725,#1832,.T.);
#4812=EDGE_CURVE('',#3736,#3728,#1833,.T.);
#4813=EDGE_CURVE('',#3735,#3736,#2488,.T.);
#4814=EDGE_CURVE('',#3737,#3735,#2489,.T.);
#4815=EDGE_CURVE('',#3738,#3736,#2490,.T.);
#4816=EDGE_CURVE('',#3737,#3738,#2491,.T.);
#4817=EDGE_CURVE('',#3739,#3737,#1834,.T.);
#4818=EDGE_CURVE('',#3740,#3738,#1835,.T.);
#4819=EDGE_CURVE('',#3739,#3740,#2492,.T.);
#4820=EDGE_CURVE('',#3733,#3739,#2493,.T.);
#4821=EDGE_CURVE('',#3734,#3740,#2494,.T.);
#4822=EDGE_CURVE('',#3741,#3742,#1836,.T.);
#4823=EDGE_CURVE('',#3742,#3743,#1837,.T.);
#4824=EDGE_CURVE('',#3743,#3744,#1838,.T.);
#4825=EDGE_CURVE('',#3744,#3741,#1839,.T.);
#4826=EDGE_CURVE('',#3745,#3746,#2495,.T.);
#4827=EDGE_CURVE('',#3717,#3745,#1840,.T.);
#4828=EDGE_CURVE('',#3747,#3720,#2496,.T.);
#4829=EDGE_CURVE('',#3746,#3747,#1841,.T.);
#4830=EDGE_CURVE('',#3721,#3742,#2497,.T.);
#4831=EDGE_CURVE('',#3743,#3724,#2498,.T.);
#4832=EDGE_CURVE('',#3744,#3723,#2499,.T.);
#4833=EDGE_CURVE('',#3741,#3722,#2500,.T.);
#4834=EDGE_CURVE('',#3745,#3707,#2501,.T.);
#4835=EDGE_CURVE('',#3746,#3706,#2502,.T.);
#4836=EDGE_CURVE('',#3747,#3704,#2503,.T.);
#4837=EDGE_CURVE('',#3748,#3749,#2006,.T.);
#4838=EDGE_CURVE('',#3750,#3748,#2504,.T.);
#4839=EDGE_CURVE('',#3750,#3751,#252,.F.);
#4840=EDGE_CURVE('',#3751,#3752,#1842,.F.);
#4841=EDGE_CURVE('',#3753,#3752,#253,.T.);
#4842=EDGE_CURVE('',#3749,#3753,#2505,.T.);
#4843=EDGE_CURVE('',#3749,#3754,#1843,.T.);
#4844=EDGE_CURVE('',#3754,#3753,#2506,.F.);
#4845=EDGE_CURVE('',#3754,#3755,#1844,.T.);
#4846=EDGE_CURVE('',#3752,#3756,#2507,.F.);
#4847=EDGE_CURVE('',#3757,#3756,#254,.F.);
#4848=EDGE_CURVE('',#3755,#3757,#2508,.T.);
#4849=EDGE_CURVE('',#3755,#3758,#1845,.T.);
#4850=EDGE_CURVE('',#3757,#3758,#2509,.T.);
#4851=EDGE_CURVE('',#3758,#3759,#2007,.T.);
#4852=EDGE_CURVE('',#3756,#3760,#1846,.F.);
#4853=EDGE_CURVE('',#3761,#3760,#255,.T.);
#4854=EDGE_CURVE('',#3759,#3761,#2510,.T.);
#4855=EDGE_CURVE('',#3759,#3762,#1847,.T.);
#4856=EDGE_CURVE('',#3762,#3761,#2511,.F.);
#4857=EDGE_CURVE('',#3762,#3763,#1848,.T.);
#4858=EDGE_CURVE('',#3760,#3764,#2512,.F.);
#4859=EDGE_CURVE('',#3765,#3764,#256,.F.);
#4860=EDGE_CURVE('',#3763,#3765,#2513,.T.);
#4861=EDGE_CURVE('',#3763,#3766,#1849,.T.);
#4862=EDGE_CURVE('',#3765,#3766,#2514,.T.);
#4863=EDGE_CURVE('',#3767,#3768,#2008,.T.);
#4864=EDGE_CURVE('',#3769,#3767,#2515,.T.);
#4865=EDGE_CURVE('',#3769,#3770,#257,.F.);
#4866=EDGE_CURVE('',#3770,#3771,#1850,.F.);
#4867=EDGE_CURVE('',#3772,#3771,#258,.T.);
#4868=EDGE_CURVE('',#3768,#3772,#2516,.T.);
#4869=EDGE_CURVE('',#3768,#3773,#1851,.T.);
#4870=EDGE_CURVE('',#3773,#3772,#2517,.F.);
#4871=EDGE_CURVE('',#3766,#3774,#2009,.T.);
#4872=EDGE_CURVE('',#3764,#3775,#1852,.F.);
#4873=EDGE_CURVE('',#3776,#3775,#259,.T.);
#4874=EDGE_CURVE('',#3774,#3776,#2518,.T.);
#4875=EDGE_CURVE('',#3774,#3777,#1853,.T.);
#4876=EDGE_CURVE('',#3777,#3776,#2519,.F.);
#4877=EDGE_CURVE('',#3778,#3748,#1854,.T.);
#4878=EDGE_CURVE('',#3778,#3750,#2520,.T.);
#4879=EDGE_CURVE('',#3773,#3779,#1855,.T.);
#4880=EDGE_CURVE('',#3771,#3751,#2521,.F.);
#4881=EDGE_CURVE('',#3779,#3778,#1856,.T.);
#4882=EDGE_CURVE('',#3780,#3767,#1857,.T.);
#4883=EDGE_CURVE('',#3780,#3769,#2522,.T.);
#4884=EDGE_CURVE('',#3777,#3780,#1858,.T.);
#4885=EDGE_CURVE('',#3775,#3770,#2523,.F.);
#4886=EDGE_CURVE('',#3781,#3781,#1859,.T.);
#4887=EDGE_CURVE('',#3781,#3782,#1860,.T.);
#4888=EDGE_CURVE('',#3782,#3782,#1861,.T.);
#4889=EDGE_CURVE('',#3783,#3783,#1862,.T.);
#4890=EDGE_CURVE('',#3784,#3784,#1863,.T.);
#4891=EDGE_CURVE('',#3784,#3782,#2524,.T.);
#4892=EDGE_CURVE('',#3785,#3785,#1864,.T.);
#4893=EDGE_CURVE('',#3785,#3784,#2525,.T.);
#4894=EDGE_CURVE('',#3786,#3786,#1865,.F.);
#4895=EDGE_CURVE('',#3786,#3785,#2526,.T.);
#4896=EDGE_CURVE('',#3779,#3787,#1866,.T.);
#4897=EDGE_CURVE('',#3788,#3787,#1867,.T.);
#4898=EDGE_CURVE('',#3787,#3788,#1868,.T.);
#4899=EDGE_CURVE('',#3783,#3788,#2527,.T.);
#4900=EDGE_CURVE('',#3789,#3790,#2010,.T.);
#4901=EDGE_CURVE('',#3791,#3789,#2528,.T.);
#4902=EDGE_CURVE('',#3791,#3792,#260,.F.);
#4903=EDGE_CURVE('',#3792,#3793,#1869,.F.);
#4904=EDGE_CURVE('',#3794,#3793,#261,.T.);
#4905=EDGE_CURVE('',#3790,#3794,#2529,.T.);
#4906=EDGE_CURVE('',#3790,#3795,#1870,.T.);
#4907=EDGE_CURVE('',#3795,#3794,#2530,.F.);
#4908=EDGE_CURVE('',#3795,#3796,#1871,.T.);
#4909=EDGE_CURVE('',#3793,#3797,#2531,.F.);
#4910=EDGE_CURVE('',#3798,#3797,#262,.F.);
#4911=EDGE_CURVE('',#3796,#3798,#2532,.T.);
#4912=EDGE_CURVE('',#3796,#3799,#1872,.T.);
#4913=EDGE_CURVE('',#3798,#3799,#2533,.T.);
#4914=EDGE_CURVE('',#3799,#3800,#2011,.T.);
#4915=EDGE_CURVE('',#3797,#3801,#1873,.F.);
#4916=EDGE_CURVE('',#3802,#3801,#263,.T.);
#4917=EDGE_CURVE('',#3800,#3802,#2534,.T.);
#4918=EDGE_CURVE('',#3800,#3803,#1874,.T.);
#4919=EDGE_CURVE('',#3803,#3802,#2535,.F.);
#4920=EDGE_CURVE('',#3803,#3804,#1875,.T.);
#4921=EDGE_CURVE('',#3801,#3805,#2536,.F.);
#4922=EDGE_CURVE('',#3806,#3805,#264,.F.);
#4923=EDGE_CURVE('',#3804,#3806,#2537,.T.);
#4924=EDGE_CURVE('',#3804,#3807,#1876,.T.);
#4925=EDGE_CURVE('',#3806,#3807,#2538,.T.);
#4926=EDGE_CURVE('',#3808,#3809,#2012,.T.);
#4927=EDGE_CURVE('',#3810,#3808,#2539,.T.);
#4928=EDGE_CURVE('',#3810,#3811,#265,.F.);
#4929=EDGE_CURVE('',#3811,#3812,#1877,.F.);
#4930=EDGE_CURVE('',#3813,#3812,#266,.T.);
#4931=EDGE_CURVE('',#3809,#3813,#2540,.T.);
#4932=EDGE_CURVE('',#3809,#3814,#1878,.T.);
#4933=EDGE_CURVE('',#3814,#3813,#2541,.F.);
#4934=EDGE_CURVE('',#3807,#3815,#2013,.T.);
#4935=EDGE_CURVE('',#3805,#3816,#1879,.F.);
#4936=EDGE_CURVE('',#3817,#3816,#267,.T.);
#4937=EDGE_CURVE('',#3815,#3817,#2542,.T.);
#4938=EDGE_CURVE('',#3815,#3818,#1880,.T.);
#4939=EDGE_CURVE('',#3818,#3817,#2543,.F.);
#4940=EDGE_CURVE('',#3819,#3789,#1881,.T.);
#4941=EDGE_CURVE('',#3819,#3791,#2544,.T.);
#4942=EDGE_CURVE('',#3814,#3820,#1882,.T.);
#4943=EDGE_CURVE('',#3812,#3792,#2545,.F.);
#4944=EDGE_CURVE('',#3820,#3819,#1883,.T.);
#4945=EDGE_CURVE('',#3821,#3808,#1884,.T.);
#4946=EDGE_CURVE('',#3821,#3810,#2546,.T.);
#4947=EDGE_CURVE('',#3818,#3821,#1885,.T.);
#4948=EDGE_CURVE('',#3816,#3811,#2547,.F.);
#4949=EDGE_CURVE('',#3822,#3822,#1886,.T.);
#4950=EDGE_CURVE('',#3822,#3823,#1887,.T.);
#4951=EDGE_CURVE('',#3823,#3823,#1888,.T.);
#4952=EDGE_CURVE('',#3824,#3824,#1889,.T.);
#4953=EDGE_CURVE('',#3825,#3825,#1890,.T.);
#4954=EDGE_CURVE('',#3825,#3823,#2548,.T.);
#4955=EDGE_CURVE('',#3826,#3826,#1891,.T.);
#4956=EDGE_CURVE('',#3826,#3825,#2549,.T.);
#4957=EDGE_CURVE('',#3827,#3827,#1892,.F.);
#4958=EDGE_CURVE('',#3827,#3826,#2550,.T.);
#4959=EDGE_CURVE('',#3820,#3828,#1893,.T.);
#4960=EDGE_CURVE('',#3829,#3828,#1894,.T.);
#4961=EDGE_CURVE('',#3828,#3829,#1895,.T.);
#4962=EDGE_CURVE('',#3824,#3829,#2551,.T.);
#4963=EDGE_CURVE('',#3830,#3831,#2014,.T.);
#4964=EDGE_CURVE('',#3832,#3830,#2552,.T.);
#4965=EDGE_CURVE('',#3832,#3833,#268,.F.);
#4966=EDGE_CURVE('',#3833,#3834,#1896,.F.);
#4967=EDGE_CURVE('',#3835,#3834,#269,.T.);
#4968=EDGE_CURVE('',#3831,#3835,#2553,.T.);
#4969=EDGE_CURVE('',#3831,#3836,#1897,.T.);
#4970=EDGE_CURVE('',#3836,#3835,#2554,.F.);
#4971=EDGE_CURVE('',#3836,#3837,#1898,.T.);
#4972=EDGE_CURVE('',#3834,#3838,#2555,.F.);
#4973=EDGE_CURVE('',#3839,#3838,#270,.F.);
#4974=EDGE_CURVE('',#3837,#3839,#2556,.T.);
#4975=EDGE_CURVE('',#3837,#3840,#1899,.T.);
#4976=EDGE_CURVE('',#3839,#3840,#2557,.T.);
#4977=EDGE_CURVE('',#3840,#3841,#2015,.T.);
#4978=EDGE_CURVE('',#3838,#3842,#1900,.F.);
#4979=EDGE_CURVE('',#3843,#3842,#271,.T.);
#4980=EDGE_CURVE('',#3841,#3843,#2558,.T.);
#4981=EDGE_CURVE('',#3841,#3844,#1901,.T.);
#4982=EDGE_CURVE('',#3844,#3843,#2559,.F.);
#4983=EDGE_CURVE('',#3844,#3845,#1902,.T.);
#4984=EDGE_CURVE('',#3842,#3846,#2560,.F.);
#4985=EDGE_CURVE('',#3847,#3846,#272,.F.);
#4986=EDGE_CURVE('',#3845,#3847,#2561,.T.);
#4987=EDGE_CURVE('',#3845,#3848,#1903,.T.);
#4988=EDGE_CURVE('',#3847,#3848,#2562,.T.);
#4989=EDGE_CURVE('',#3849,#3850,#2016,.T.);
#4990=EDGE_CURVE('',#3851,#3849,#2563,.T.);
#4991=EDGE_CURVE('',#3851,#3852,#273,.F.);
#4992=EDGE_CURVE('',#3852,#3853,#1904,.F.);
#4993=EDGE_CURVE('',#3854,#3853,#274,.T.);
#4994=EDGE_CURVE('',#3850,#3854,#2564,.T.);
#4995=EDGE_CURVE('',#3850,#3855,#1905,.T.);
#4996=EDGE_CURVE('',#3855,#3854,#2565,.F.);
#4997=EDGE_CURVE('',#3848,#3856,#2017,.T.);
#4998=EDGE_CURVE('',#3846,#3857,#1906,.F.);
#4999=EDGE_CURVE('',#3858,#3857,#275,.T.);
#5000=EDGE_CURVE('',#3856,#3858,#2566,.T.);
#5001=EDGE_CURVE('',#3856,#3859,#1907,.T.);
#5002=EDGE_CURVE('',#3859,#3858,#2567,.F.);
#5003=EDGE_CURVE('',#3860,#3830,#1908,.T.);
#5004=EDGE_CURVE('',#3860,#3832,#2568,.T.);
#5005=EDGE_CURVE('',#3855,#3861,#1909,.T.);
#5006=EDGE_CURVE('',#3853,#3833,#2569,.F.);
#5007=EDGE_CURVE('',#3861,#3860,#1910,.T.);
#5008=EDGE_CURVE('',#3862,#3849,#1911,.T.);
#5009=EDGE_CURVE('',#3862,#3851,#2570,.T.);
#5010=EDGE_CURVE('',#3859,#3862,#1912,.T.);
#5011=EDGE_CURVE('',#3857,#3852,#2571,.F.);
#5012=EDGE_CURVE('',#3863,#3863,#1913,.T.);
#5013=EDGE_CURVE('',#3863,#3864,#1914,.T.);
#5014=EDGE_CURVE('',#3864,#3864,#1915,.T.);
#5015=EDGE_CURVE('',#3865,#3865,#1916,.T.);
#5016=EDGE_CURVE('',#3866,#3866,#1917,.T.);
#5017=EDGE_CURVE('',#3866,#3864,#2572,.T.);
#5018=EDGE_CURVE('',#3867,#3867,#1918,.T.);
#5019=EDGE_CURVE('',#3867,#3866,#2573,.T.);
#5020=EDGE_CURVE('',#3868,#3868,#1919,.F.);
#5021=EDGE_CURVE('',#3868,#3867,#2574,.T.);
#5022=EDGE_CURVE('',#3861,#3869,#1920,.T.);
#5023=EDGE_CURVE('',#3870,#3869,#1921,.T.);
#5024=EDGE_CURVE('',#3869,#3870,#1922,.T.);
#5025=EDGE_CURVE('',#3865,#3870,#2575,.T.);
#5026=EDGE_CURVE('',#3871,#3872,#2018,.T.);
#5027=EDGE_CURVE('',#3873,#3871,#2576,.T.);
#5028=EDGE_CURVE('',#3873,#3874,#276,.F.);
#5029=EDGE_CURVE('',#3874,#3875,#1923,.F.);
#5030=EDGE_CURVE('',#3876,#3875,#277,.T.);
#5031=EDGE_CURVE('',#3872,#3876,#2577,.T.);
#5032=EDGE_CURVE('',#3872,#3877,#1924,.T.);
#5033=EDGE_CURVE('',#3877,#3876,#2578,.F.);
#5034=EDGE_CURVE('',#3877,#3878,#1925,.T.);
#5035=EDGE_CURVE('',#3875,#3879,#2579,.F.);
#5036=EDGE_CURVE('',#3880,#3879,#278,.F.);
#5037=EDGE_CURVE('',#3878,#3880,#2580,.T.);
#5038=EDGE_CURVE('',#3878,#3881,#1926,.T.);
#5039=EDGE_CURVE('',#3880,#3881,#2581,.T.);
#5040=EDGE_CURVE('',#3881,#3882,#2019,.T.);
#5041=EDGE_CURVE('',#3879,#3883,#1927,.F.);
#5042=EDGE_CURVE('',#3884,#3883,#279,.T.);
#5043=EDGE_CURVE('',#3882,#3884,#2582,.T.);
#5044=EDGE_CURVE('',#3882,#3885,#1928,.T.);
#5045=EDGE_CURVE('',#3885,#3884,#2583,.F.);
#5046=EDGE_CURVE('',#3885,#3886,#1929,.T.);
#5047=EDGE_CURVE('',#3883,#3887,#2584,.F.);
#5048=EDGE_CURVE('',#3888,#3887,#280,.F.);
#5049=EDGE_CURVE('',#3886,#3888,#2585,.T.);
#5050=EDGE_CURVE('',#3886,#3889,#1930,.T.);
#5051=EDGE_CURVE('',#3888,#3889,#2586,.T.);
#5052=EDGE_CURVE('',#3890,#3891,#2020,.T.);
#5053=EDGE_CURVE('',#3892,#3890,#2587,.T.);
#5054=EDGE_CURVE('',#3892,#3893,#281,.F.);
#5055=EDGE_CURVE('',#3893,#3894,#1931,.F.);
#5056=EDGE_CURVE('',#3895,#3894,#282,.T.);
#5057=EDGE_CURVE('',#3891,#3895,#2588,.T.);
#5058=EDGE_CURVE('',#3891,#3896,#1932,.T.);
#5059=EDGE_CURVE('',#3896,#3895,#2589,.F.);
#5060=EDGE_CURVE('',#3889,#3897,#2021,.T.);
#5061=EDGE_CURVE('',#3887,#3898,#1933,.F.);
#5062=EDGE_CURVE('',#3899,#3898,#283,.T.);
#5063=EDGE_CURVE('',#3897,#3899,#2590,.T.);
#5064=EDGE_CURVE('',#3897,#3900,#1934,.T.);
#5065=EDGE_CURVE('',#3900,#3899,#2591,.F.);
#5066=EDGE_CURVE('',#3901,#3871,#1935,.T.);
#5067=EDGE_CURVE('',#3901,#3873,#2592,.T.);
#5068=EDGE_CURVE('',#3896,#3902,#1936,.T.);
#5069=EDGE_CURVE('',#3894,#3874,#2593,.F.);
#5070=EDGE_CURVE('',#3902,#3901,#1937,.T.);
#5071=EDGE_CURVE('',#3903,#3890,#1938,.T.);
#5072=EDGE_CURVE('',#3903,#3892,#2594,.T.);
#5073=EDGE_CURVE('',#3900,#3903,#1939,.T.);
#5074=EDGE_CURVE('',#3898,#3893,#2595,.F.);
#5075=EDGE_CURVE('',#3904,#3904,#1940,.T.);
#5076=EDGE_CURVE('',#3904,#3905,#1941,.T.);
#5077=EDGE_CURVE('',#3905,#3905,#1942,.T.);
#5078=EDGE_CURVE('',#3906,#3906,#1943,.T.);
#5079=EDGE_CURVE('',#3907,#3907,#1944,.T.);
#5080=EDGE_CURVE('',#3907,#3905,#2596,.T.);
#5081=EDGE_CURVE('',#3908,#3908,#1945,.T.);
#5082=EDGE_CURVE('',#3908,#3907,#2597,.T.);
#5083=EDGE_CURVE('',#3909,#3909,#1946,.F.);
#5084=EDGE_CURVE('',#3909,#3908,#2598,.T.);
#5085=EDGE_CURVE('',#3902,#3910,#1947,.T.);
#5086=EDGE_CURVE('',#3911,#3910,#1948,.T.);
#5087=EDGE_CURVE('',#3910,#3911,#1949,.T.);
#5088=EDGE_CURVE('',#3906,#3911,#2599,.T.);
#5089=ORIENTED_EDGE('',*,*,#3912,.T.);
#5090=ORIENTED_EDGE('',*,*,#3913,.T.);
#5091=ORIENTED_EDGE('',*,*,#3914,.T.);
#5092=ORIENTED_EDGE('',*,*,#3915,.F.);
#5093=ORIENTED_EDGE('',*,*,#3916,.T.);
#5094=ORIENTED_EDGE('',*,*,#3917,.T.);
#5095=ORIENTED_EDGE('',*,*,#3918,.F.);
#5096=ORIENTED_EDGE('',*,*,#3919,.T.);
#5097=ORIENTED_EDGE('',*,*,#3920,.T.);
#5098=ORIENTED_EDGE('',*,*,#3921,.T.);
#5099=ORIENTED_EDGE('',*,*,#3915,.T.);
#5100=ORIENTED_EDGE('',*,*,#3922,.F.);
#5101=ORIENTED_EDGE('',*,*,#3923,.F.);
#5102=ORIENTED_EDGE('',*,*,#3924,.T.);
#5103=ORIENTED_EDGE('',*,*,#3912,.F.);
#5104=ORIENTED_EDGE('',*,*,#3925,.F.);
#5105=ORIENTED_EDGE('',*,*,#3926,.F.);
#5106=ORIENTED_EDGE('',*,*,#3927,.F.);
#5107=ORIENTED_EDGE('',*,*,#3928,.T.);
#5108=ORIENTED_EDGE('',*,*,#3913,.F.);
#5109=ORIENTED_EDGE('',*,*,#3924,.F.);
#5110=ORIENTED_EDGE('',*,*,#3929,.F.);
#5111=ORIENTED_EDGE('',*,*,#3930,.T.);
#5112=ORIENTED_EDGE('',*,*,#3931,.F.);
#5113=ORIENTED_EDGE('',*,*,#3919,.F.);
#5114=ORIENTED_EDGE('',*,*,#3914,.F.);
#5115=ORIENTED_EDGE('',*,*,#3928,.F.);
#5116=ORIENTED_EDGE('',*,*,#3932,.F.);
#5117=ORIENTED_EDGE('',*,*,#3933,.T.);
#5118=ORIENTED_EDGE('',*,*,#3934,.F.);
#5119=ORIENTED_EDGE('',*,*,#3930,.F.);
#5120=ORIENTED_EDGE('',*,*,#3935,.F.);
#5121=ORIENTED_EDGE('',*,*,#3936,.F.);
#5122=ORIENTED_EDGE('',*,*,#3933,.F.);
#5123=ORIENTED_EDGE('',*,*,#3937,.F.);
#5124=ORIENTED_EDGE('',*,*,#3926,.T.);
#5125=ORIENTED_EDGE('',*,*,#3938,.F.);
#5126=ORIENTED_EDGE('',*,*,#3939,.T.);
#5127=ORIENTED_EDGE('',*,*,#3940,.F.);
#5128=ORIENTED_EDGE('',*,*,#3931,.T.);
#5129=ORIENTED_EDGE('',*,*,#3934,.T.);
#5130=ORIENTED_EDGE('',*,*,#3936,.T.);
#5131=ORIENTED_EDGE('',*,*,#3941,.F.);
#5132=ORIENTED_EDGE('',*,*,#3942,.T.);
#5133=ORIENTED_EDGE('',*,*,#3943,.F.);
#5134=ORIENTED_EDGE('',*,*,#3944,.F.);
#5135=ORIENTED_EDGE('',*,*,#3945,.T.);
#5136=ORIENTED_EDGE('',*,*,#3920,.F.);
#5137=ORIENTED_EDGE('',*,*,#3935,.T.);
#5138=ORIENTED_EDGE('',*,*,#3946,.F.);
#5139=ORIENTED_EDGE('',*,*,#3947,.F.);
#5140=ORIENTED_EDGE('',*,*,#3948,.F.);
#5141=ORIENTED_EDGE('',*,*,#3949,.F.);
#5142=ORIENTED_EDGE('',*,*,#3950,.F.);
#5143=ORIENTED_EDGE('',*,*,#3951,.T.);
#5144=ORIENTED_EDGE('',*,*,#3952,.T.);
#5145=ORIENTED_EDGE('',*,*,#3953,.T.);
#5146=ORIENTED_EDGE('',*,*,#3954,.T.);
#5147=ORIENTED_EDGE('',*,*,#3955,.T.);
#5148=ORIENTED_EDGE('',*,*,#3956,.T.);
#5149=ORIENTED_EDGE('',*,*,#3957,.T.);
#5150=ORIENTED_EDGE('',*,*,#3958,.T.);
#5151=ORIENTED_EDGE('',*,*,#3941,.T.);
#5152=ORIENTED_EDGE('',*,*,#3959,.T.);
#5153=ORIENTED_EDGE('',*,*,#3960,.T.);
#5154=ORIENTED_EDGE('',*,*,#3961,.T.);
#5155=ORIENTED_EDGE('',*,*,#3962,.T.);
#5156=ORIENTED_EDGE('',*,*,#3963,.T.);
#5157=ORIENTED_EDGE('',*,*,#3964,.T.);
#5158=ORIENTED_EDGE('',*,*,#3965,.T.);
#5159=ORIENTED_EDGE('',*,*,#3966,.T.);
#5160=ORIENTED_EDGE('',*,*,#3967,.T.);
#5161=ORIENTED_EDGE('',*,*,#3968,.T.);
#5162=ORIENTED_EDGE('',*,*,#3969,.T.);
#5163=ORIENTED_EDGE('',*,*,#3966,.F.);
#5164=ORIENTED_EDGE('',*,*,#3970,.T.);
#5165=ORIENTED_EDGE('',*,*,#3971,.T.);
#5166=ORIENTED_EDGE('',*,*,#3972,.T.);
#5167=ORIENTED_EDGE('',*,*,#3973,.T.);
#5168=ORIENTED_EDGE('',*,*,#3974,.T.);
#5169=ORIENTED_EDGE('',*,*,#3975,.T.);
#5170=ORIENTED_EDGE('',*,*,#3972,.F.);
#5171=ORIENTED_EDGE('',*,*,#3976,.T.);
#5172=ORIENTED_EDGE('',*,*,#3977,.T.);
#5173=ORIENTED_EDGE('',*,*,#3974,.F.);
#5174=ORIENTED_EDGE('',*,*,#3978,.T.);
#5175=ORIENTED_EDGE('',*,*,#3968,.F.);
#5176=ORIENTED_EDGE('',*,*,#3979,.T.);
#5177=ORIENTED_EDGE('',*,*,#3980,.T.);
#5178=ORIENTED_EDGE('',*,*,#3964,.F.);
#5179=ORIENTED_EDGE('',*,*,#3981,.T.);
#5180=ORIENTED_EDGE('',*,*,#3982,.T.);
#5181=ORIENTED_EDGE('',*,*,#3983,.T.);
#5182=ORIENTED_EDGE('',*,*,#3979,.F.);
#5183=ORIENTED_EDGE('',*,*,#3984,.T.);
#5184=ORIENTED_EDGE('',*,*,#3970,.F.);
#5185=ORIENTED_EDGE('',*,*,#3985,.T.);
#5186=ORIENTED_EDGE('',*,*,#3959,.F.);
#5187=ORIENTED_EDGE('',*,*,#3986,.T.);
#5188=ORIENTED_EDGE('',*,*,#3987,.T.);
#5189=ORIENTED_EDGE('',*,*,#3988,.T.);
#5190=ORIENTED_EDGE('',*,*,#3989,.T.);
#5191=ORIENTED_EDGE('',*,*,#3986,.F.);
#5192=ORIENTED_EDGE('',*,*,#3990,.T.);
#5193=ORIENTED_EDGE('',*,*,#3982,.F.);
#5194=ORIENTED_EDGE('',*,*,#3991,.T.);
#5195=ORIENTED_EDGE('',*,*,#3960,.F.);
#5196=ORIENTED_EDGE('',*,*,#3992,.F.);
#5197=ORIENTED_EDGE('',*,*,#3993,.F.);
#5198=ORIENTED_EDGE('',*,*,#3994,.T.);
#5199=ORIENTED_EDGE('',*,*,#3995,.F.);
#5200=ORIENTED_EDGE('',*,*,#3996,.F.);
#5201=ORIENTED_EDGE('',*,*,#3997,.F.);
#5202=ORIENTED_EDGE('',*,*,#3948,.T.);
#5203=ORIENTED_EDGE('',*,*,#3998,.T.);
#5204=ORIENTED_EDGE('',*,*,#3985,.F.);
#5205=ORIENTED_EDGE('',*,*,#3999,.T.);
#5206=ORIENTED_EDGE('',*,*,#4000,.T.);
#5207=ORIENTED_EDGE('',*,*,#3992,.T.);
#5208=ORIENTED_EDGE('',*,*,#3973,.F.);
#5209=ORIENTED_EDGE('',*,*,#3975,.F.);
#5210=ORIENTED_EDGE('',*,*,#3977,.F.);
#5211=ORIENTED_EDGE('',*,*,#3967,.F.);
#5212=ORIENTED_EDGE('',*,*,#3965,.F.);
#5213=ORIENTED_EDGE('',*,*,#3980,.F.);
#5214=ORIENTED_EDGE('',*,*,#3983,.F.);
#5215=ORIENTED_EDGE('',*,*,#4001,.F.);
#5216=ORIENTED_EDGE('',*,*,#4002,.F.);
#5217=ORIENTED_EDGE('',*,*,#4003,.F.);
#5218=ORIENTED_EDGE('',*,*,#4004,.F.);
#5219=ORIENTED_EDGE('',*,*,#4005,.F.);
#5220=ORIENTED_EDGE('',*,*,#4006,.F.);
#5221=ORIENTED_EDGE('',*,*,#4007,.F.);
#5222=ORIENTED_EDGE('',*,*,#4008,.F.);
#5223=ORIENTED_EDGE('',*,*,#4009,.F.);
#5224=ORIENTED_EDGE('',*,*,#4010,.F.);
#5225=ORIENTED_EDGE('',*,*,#4011,.F.);
#5226=ORIENTED_EDGE('',*,*,#4012,.F.);
#5227=ORIENTED_EDGE('',*,*,#3999,.F.);
#5228=ORIENTED_EDGE('',*,*,#3990,.F.);
#5229=ORIENTED_EDGE('',*,*,#4013,.T.);
#5230=ORIENTED_EDGE('',*,*,#4014,.T.);
#5231=ORIENTED_EDGE('',*,*,#4001,.T.);
#5232=ORIENTED_EDGE('',*,*,#3989,.F.);
#5233=ORIENTED_EDGE('',*,*,#4015,.T.);
#5234=ORIENTED_EDGE('',*,*,#4016,.F.);
#5235=ORIENTED_EDGE('',*,*,#4017,.T.);
#5236=ORIENTED_EDGE('',*,*,#4018,.T.);
#5237=ORIENTED_EDGE('',*,*,#4019,.T.);
#5238=ORIENTED_EDGE('',*,*,#4020,.F.);
#5239=ORIENTED_EDGE('',*,*,#4013,.F.);
#5240=ORIENTED_EDGE('',*,*,#4021,.F.);
#5241=ORIENTED_EDGE('',*,*,#4022,.F.);
#5242=ORIENTED_EDGE('',*,*,#4023,.F.);
#5243=ORIENTED_EDGE('',*,*,#4024,.F.);
#5244=ORIENTED_EDGE('',*,*,#4025,.F.);
#5245=ORIENTED_EDGE('',*,*,#4026,.F.);
#5246=ORIENTED_EDGE('',*,*,#4027,.F.);
#5247=ORIENTED_EDGE('',*,*,#4028,.T.);
#5248=ORIENTED_EDGE('',*,*,#4029,.F.);
#5249=ORIENTED_EDGE('',*,*,#4028,.F.);
#5250=ORIENTED_EDGE('',*,*,#4030,.F.);
#5251=ORIENTED_EDGE('',*,*,#4022,.T.);
#5252=ORIENTED_EDGE('',*,*,#4031,.F.);
#5253=ORIENTED_EDGE('',*,*,#3951,.F.);
#5254=ORIENTED_EDGE('',*,*,#4032,.F.);
#5255=ORIENTED_EDGE('',*,*,#4033,.T.);
#5256=ORIENTED_EDGE('',*,*,#4034,.F.);
#5257=ORIENTED_EDGE('',*,*,#4033,.F.);
#5258=ORIENTED_EDGE('',*,*,#4035,.F.);
#5259=ORIENTED_EDGE('',*,*,#4026,.T.);
#5260=ORIENTED_EDGE('',*,*,#4023,.T.);
#5261=ORIENTED_EDGE('',*,*,#4030,.T.);
#5262=ORIENTED_EDGE('',*,*,#4027,.T.);
#5263=ORIENTED_EDGE('',*,*,#4035,.T.);
#5264=ORIENTED_EDGE('',*,*,#4032,.T.);
#5265=ORIENTED_EDGE('',*,*,#3950,.T.);
#5266=ORIENTED_EDGE('',*,*,#4036,.F.);
#5267=ORIENTED_EDGE('',*,*,#4037,.F.);
#5268=ORIENTED_EDGE('',*,*,#4038,.F.);
#5269=ORIENTED_EDGE('',*,*,#4039,.T.);
#5270=ORIENTED_EDGE('',*,*,#3922,.T.);
#5271=ORIENTED_EDGE('',*,*,#3940,.T.);
#5272=ORIENTED_EDGE('',*,*,#4040,.T.);
#5273=ORIENTED_EDGE('',*,*,#4041,.T.);
#5274=ORIENTED_EDGE('',*,*,#4042,.T.);
#5275=ORIENTED_EDGE('',*,*,#4043,.T.);
#5276=ORIENTED_EDGE('',*,*,#4044,.T.);
#5277=ORIENTED_EDGE('',*,*,#4045,.T.);
#5278=ORIENTED_EDGE('',*,*,#4046,.T.);
#5279=ORIENTED_EDGE('',*,*,#4024,.T.);
#5280=ORIENTED_EDGE('',*,*,#4039,.F.);
#5281=ORIENTED_EDGE('',*,*,#4047,.F.);
#5282=ORIENTED_EDGE('',*,*,#4048,.F.);
#5283=ORIENTED_EDGE('',*,*,#4049,.F.);
#5284=ORIENTED_EDGE('',*,*,#4050,.F.);
#5285=ORIENTED_EDGE('',*,*,#4051,.F.);
#5286=ORIENTED_EDGE('',*,*,#4017,.F.);
#5287=ORIENTED_EDGE('',*,*,#4052,.F.);
#5288=ORIENTED_EDGE('',*,*,#4053,.F.);
#5289=ORIENTED_EDGE('',*,*,#4054,.F.);
#5290=ORIENTED_EDGE('',*,*,#4055,.T.);
#5291=ORIENTED_EDGE('',*,*,#4056,.F.);
#5292=ORIENTED_EDGE('',*,*,#4057,.F.);
#5293=ORIENTED_EDGE('',*,*,#4042,.F.);
#5294=ORIENTED_EDGE('',*,*,#4058,.F.);
#5295=ORIENTED_EDGE('',*,*,#4059,.F.);
#5296=ORIENTED_EDGE('',*,*,#4055,.F.);
#5297=ORIENTED_EDGE('',*,*,#4060,.F.);
#5298=ORIENTED_EDGE('',*,*,#4061,.T.);
#5299=ORIENTED_EDGE('',*,*,#4062,.F.);
#5300=ORIENTED_EDGE('',*,*,#4063,.F.);
#5301=ORIENTED_EDGE('',*,*,#4040,.F.);
#5302=ORIENTED_EDGE('',*,*,#3939,.F.);
#5303=ORIENTED_EDGE('',*,*,#4064,.F.);
#5304=ORIENTED_EDGE('',*,*,#4061,.F.);
#5305=ORIENTED_EDGE('',*,*,#4065,.F.);
#5306=ORIENTED_EDGE('',*,*,#4066,.T.);
#5307=ORIENTED_EDGE('',*,*,#3954,.F.);
#5308=ORIENTED_EDGE('',*,*,#4067,.F.);
#5309=ORIENTED_EDGE('',*,*,#4068,.F.);
#5310=ORIENTED_EDGE('',*,*,#4069,.F.);
#5311=ORIENTED_EDGE('',*,*,#3955,.F.);
#5312=ORIENTED_EDGE('',*,*,#4066,.F.);
#5313=ORIENTED_EDGE('',*,*,#4070,.F.);
#5314=ORIENTED_EDGE('',*,*,#4071,.T.);
#5315=ORIENTED_EDGE('',*,*,#3957,.F.);
#5316=ORIENTED_EDGE('',*,*,#4072,.F.);
#5317=ORIENTED_EDGE('',*,*,#4073,.F.);
#5318=ORIENTED_EDGE('',*,*,#3942,.F.);
#5319=ORIENTED_EDGE('',*,*,#3958,.F.);
#5320=ORIENTED_EDGE('',*,*,#4071,.F.);
#5321=ORIENTED_EDGE('',*,*,#4057,.T.);
#5322=ORIENTED_EDGE('',*,*,#4074,.T.);
#5323=ORIENTED_EDGE('',*,*,#4075,.F.);
#5324=ORIENTED_EDGE('',*,*,#4043,.F.);
#5325=ORIENTED_EDGE('',*,*,#3925,.T.);
#5326=ORIENTED_EDGE('',*,*,#3918,.T.);
#5327=ORIENTED_EDGE('',*,*,#4076,.T.);
#5328=ORIENTED_EDGE('',*,*,#4077,.T.);
#5329=ORIENTED_EDGE('',*,*,#4062,.T.);
#5330=ORIENTED_EDGE('',*,*,#4064,.T.);
#5331=ORIENTED_EDGE('',*,*,#3938,.T.);
#5332=ORIENTED_EDGE('',*,*,#4068,.T.);
#5333=ORIENTED_EDGE('',*,*,#4078,.T.);
#5334=ORIENTED_EDGE('',*,*,#4079,.T.);
#5335=ORIENTED_EDGE('',*,*,#4080,.T.);
#5336=ORIENTED_EDGE('',*,*,#4081,.T.);
#5337=ORIENTED_EDGE('',*,*,#4082,.T.);
#5338=ORIENTED_EDGE('',*,*,#4067,.T.);
#5339=ORIENTED_EDGE('',*,*,#3953,.F.);
#5340=ORIENTED_EDGE('',*,*,#4083,.T.);
#5341=ORIENTED_EDGE('',*,*,#4084,.F.);
#5342=ORIENTED_EDGE('',*,*,#4085,.F.);
#5343=ORIENTED_EDGE('',*,*,#4078,.F.);
#5344=ORIENTED_EDGE('',*,*,#4069,.T.);
#5345=ORIENTED_EDGE('',*,*,#4082,.F.);
#5346=ORIENTED_EDGE('',*,*,#4086,.T.);
#5347=ORIENTED_EDGE('',*,*,#4087,.F.);
#5348=ORIENTED_EDGE('',*,*,#4088,.F.);
#5349=ORIENTED_EDGE('',*,*,#4089,.F.);
#5350=ORIENTED_EDGE('',*,*,#4072,.T.);
#5351=ORIENTED_EDGE('',*,*,#3956,.F.);
#5352=ORIENTED_EDGE('',*,*,#4090,.F.);
#5353=ORIENTED_EDGE('',*,*,#4091,.T.);
#5354=ORIENTED_EDGE('',*,*,#4079,.F.);
#5355=ORIENTED_EDGE('',*,*,#4085,.T.);
#5356=ORIENTED_EDGE('',*,*,#4021,.T.);
#5357=ORIENTED_EDGE('',*,*,#4046,.F.);
#5358=ORIENTED_EDGE('',*,*,#4092,.T.);
#5359=ORIENTED_EDGE('',*,*,#4093,.F.);
#5360=ORIENTED_EDGE('',*,*,#4083,.F.);
#5361=ORIENTED_EDGE('',*,*,#3952,.F.);
#5362=ORIENTED_EDGE('',*,*,#4031,.T.);
#5363=ORIENTED_EDGE('',*,*,#4034,.T.);
#5364=ORIENTED_EDGE('',*,*,#4025,.T.);
#5365=ORIENTED_EDGE('',*,*,#4029,.T.);
#5366=ORIENTED_EDGE('',*,*,#4094,.T.);
#5367=ORIENTED_EDGE('',*,*,#4095,.T.);
#5368=ORIENTED_EDGE('',*,*,#4096,.T.);
#5369=ORIENTED_EDGE('',*,*,#4097,.F.);
#5370=ORIENTED_EDGE('',*,*,#3916,.F.);
#5371=ORIENTED_EDGE('',*,*,#3921,.F.);
#5372=ORIENTED_EDGE('',*,*,#3945,.F.);
#5373=ORIENTED_EDGE('',*,*,#4098,.F.);
#5374=ORIENTED_EDGE('',*,*,#4099,.F.);
#5375=ORIENTED_EDGE('',*,*,#4100,.F.);
#5376=ORIENTED_EDGE('',*,*,#4087,.T.);
#5377=ORIENTED_EDGE('',*,*,#4101,.T.);
#5378=ORIENTED_EDGE('',*,*,#4102,.T.);
#5379=ORIENTED_EDGE('',*,*,#4090,.T.);
#5380=ORIENTED_EDGE('',*,*,#4084,.T.);
#5381=ORIENTED_EDGE('',*,*,#4093,.T.);
#5382=ORIENTED_EDGE('',*,*,#4103,.T.);
#5383=ORIENTED_EDGE('',*,*,#4104,.T.);
#5384=ORIENTED_EDGE('',*,*,#4103,.F.);
#5385=ORIENTED_EDGE('',*,*,#4092,.F.);
#5386=ORIENTED_EDGE('',*,*,#4045,.F.);
#5387=ORIENTED_EDGE('',*,*,#4105,.T.);
#5388=ORIENTED_EDGE('',*,*,#4104,.F.);
#5389=ORIENTED_EDGE('',*,*,#4105,.F.);
#5390=ORIENTED_EDGE('',*,*,#4044,.F.);
#5391=ORIENTED_EDGE('',*,*,#4075,.T.);
#5392=ORIENTED_EDGE('',*,*,#4106,.T.);
#5393=ORIENTED_EDGE('',*,*,#4107,.T.);
#5394=ORIENTED_EDGE('',*,*,#4094,.F.);
#5395=ORIENTED_EDGE('',*,*,#4107,.F.);
#5396=ORIENTED_EDGE('',*,*,#4108,.F.);
#5397=ORIENTED_EDGE('',*,*,#4109,.F.);
#5398=ORIENTED_EDGE('',*,*,#4101,.F.);
#5399=ORIENTED_EDGE('',*,*,#4086,.F.);
#5400=ORIENTED_EDGE('',*,*,#4081,.F.);
#5401=ORIENTED_EDGE('',*,*,#4110,.F.);
#5402=ORIENTED_EDGE('',*,*,#4095,.F.);
#5403=ORIENTED_EDGE('',*,*,#4109,.T.);
#5404=ORIENTED_EDGE('',*,*,#4111,.F.);
#5405=ORIENTED_EDGE('',*,*,#4112,.T.);
#5406=ORIENTED_EDGE('',*,*,#4056,.T.);
#5407=ORIENTED_EDGE('',*,*,#4059,.T.);
#5408=ORIENTED_EDGE('',*,*,#4113,.T.);
#5409=ORIENTED_EDGE('',*,*,#4111,.T.);
#5410=ORIENTED_EDGE('',*,*,#4108,.T.);
#5411=ORIENTED_EDGE('',*,*,#4106,.F.);
#5412=ORIENTED_EDGE('',*,*,#4074,.F.);
#5413=ORIENTED_EDGE('',*,*,#4058,.T.);
#5414=ORIENTED_EDGE('',*,*,#4041,.F.);
#5415=ORIENTED_EDGE('',*,*,#4063,.T.);
#5416=ORIENTED_EDGE('',*,*,#4077,.F.);
#5417=ORIENTED_EDGE('',*,*,#4114,.F.);
#5418=ORIENTED_EDGE('',*,*,#4096,.F.);
#5419=ORIENTED_EDGE('',*,*,#4112,.F.);
#5420=ORIENTED_EDGE('',*,*,#4113,.F.);
#5421=ORIENTED_EDGE('',*,*,#4102,.F.);
#5422=ORIENTED_EDGE('',*,*,#4110,.T.);
#5423=ORIENTED_EDGE('',*,*,#4080,.F.);
#5424=ORIENTED_EDGE('',*,*,#4091,.F.);
#5425=ORIENTED_EDGE('',*,*,#4088,.T.);
#5426=ORIENTED_EDGE('',*,*,#4100,.T.);
#5427=ORIENTED_EDGE('',*,*,#4115,.T.);
#5428=ORIENTED_EDGE('',*,*,#4116,.F.);
#5429=ORIENTED_EDGE('',*,*,#4098,.T.);
#5430=ORIENTED_EDGE('',*,*,#3944,.T.);
#5431=ORIENTED_EDGE('',*,*,#4117,.F.);
#5432=ORIENTED_EDGE('',*,*,#4118,.F.);
#5433=ORIENTED_EDGE('',*,*,#4099,.T.);
#5434=ORIENTED_EDGE('',*,*,#4118,.T.);
#5435=ORIENTED_EDGE('',*,*,#4119,.F.);
#5436=ORIENTED_EDGE('',*,*,#4115,.F.);
#5437=ORIENTED_EDGE('',*,*,#4073,.T.);
#5438=ORIENTED_EDGE('',*,*,#4089,.T.);
#5439=ORIENTED_EDGE('',*,*,#4116,.T.);
#5440=ORIENTED_EDGE('',*,*,#4119,.T.);
#5441=ORIENTED_EDGE('',*,*,#4117,.T.);
#5442=ORIENTED_EDGE('',*,*,#3943,.T.);
#5443=ORIENTED_EDGE('',*,*,#4097,.T.);
#5444=ORIENTED_EDGE('',*,*,#4114,.T.);
#5445=ORIENTED_EDGE('',*,*,#4076,.F.);
#5446=ORIENTED_EDGE('',*,*,#3917,.F.);
#5447=ORIENTED_EDGE('',*,*,#4120,.T.);
#5448=ORIENTED_EDGE('',*,*,#4121,.T.);
#5449=ORIENTED_EDGE('',*,*,#4122,.T.);
#5450=ORIENTED_EDGE('',*,*,#4010,.T.);
#5451=ORIENTED_EDGE('',*,*,#4123,.T.);
#5452=ORIENTED_EDGE('',*,*,#4011,.T.);
#5453=ORIENTED_EDGE('',*,*,#4122,.F.);
#5454=ORIENTED_EDGE('',*,*,#4124,.T.);
#5455=ORIENTED_EDGE('',*,*,#4125,.T.);
#5456=ORIENTED_EDGE('',*,*,#4012,.T.);
#5457=ORIENTED_EDGE('',*,*,#4123,.F.);
#5458=ORIENTED_EDGE('',*,*,#4126,.T.);
#5459=ORIENTED_EDGE('',*,*,#4127,.T.);
#5460=ORIENTED_EDGE('',*,*,#4128,.T.);
#5461=ORIENTED_EDGE('',*,*,#4129,.T.);
#5462=ORIENTED_EDGE('',*,*,#4004,.T.);
#5463=ORIENTED_EDGE('',*,*,#4130,.T.);
#5464=ORIENTED_EDGE('',*,*,#4005,.T.);
#5465=ORIENTED_EDGE('',*,*,#4129,.F.);
#5466=ORIENTED_EDGE('',*,*,#4131,.T.);
#5467=ORIENTED_EDGE('',*,*,#4132,.T.);
#5468=ORIENTED_EDGE('',*,*,#4006,.T.);
#5469=ORIENTED_EDGE('',*,*,#4130,.F.);
#5470=ORIENTED_EDGE('',*,*,#4133,.T.);
#5471=ORIENTED_EDGE('',*,*,#4134,.T.);
#5472=ORIENTED_EDGE('',*,*,#4007,.T.);
#5473=ORIENTED_EDGE('',*,*,#4132,.F.);
#5474=ORIENTED_EDGE('',*,*,#4037,.T.);
#5475=ORIENTED_EDGE('',*,*,#4135,.T.);
#5476=ORIENTED_EDGE('',*,*,#4008,.T.);
#5477=ORIENTED_EDGE('',*,*,#4134,.F.);
#5478=ORIENTED_EDGE('',*,*,#4136,.T.);
#5479=ORIENTED_EDGE('',*,*,#4137,.T.);
#5480=ORIENTED_EDGE('',*,*,#4009,.T.);
#5481=ORIENTED_EDGE('',*,*,#4135,.F.);
#5482=ORIENTED_EDGE('',*,*,#3996,.T.);
#5483=ORIENTED_EDGE('',*,*,#4138,.T.);
#5484=ORIENTED_EDGE('',*,*,#4139,.T.);
#5485=ORIENTED_EDGE('',*,*,#4140,.T.);
#5486=ORIENTED_EDGE('',*,*,#4002,.T.);
#5487=ORIENTED_EDGE('',*,*,#4141,.T.);
#5488=ORIENTED_EDGE('',*,*,#4003,.T.);
#5489=ORIENTED_EDGE('',*,*,#4140,.F.);
#5490=ORIENTED_EDGE('',*,*,#4142,.T.);
#5491=ORIENTED_EDGE('',*,*,#4014,.F.);
#5492=ORIENTED_EDGE('',*,*,#4143,.T.);
#5493=ORIENTED_EDGE('',*,*,#4138,.F.);
#5494=ORIENTED_EDGE('',*,*,#4141,.F.);
#5495=ORIENTED_EDGE('',*,*,#4144,.T.);
#5496=ORIENTED_EDGE('',*,*,#4127,.F.);
#5497=ORIENTED_EDGE('',*,*,#4137,.F.);
#5498=ORIENTED_EDGE('',*,*,#4145,.T.);
#5499=ORIENTED_EDGE('',*,*,#4120,.F.);
#5500=ORIENTED_EDGE('',*,*,#4125,.F.);
#5501=ORIENTED_EDGE('',*,*,#4146,.T.);
#5502=ORIENTED_EDGE('',*,*,#4000,.F.);
#5503=ORIENTED_EDGE('',*,*,#4146,.F.);
#5504=ORIENTED_EDGE('',*,*,#4147,.T.);
#5505=ORIENTED_EDGE('',*,*,#4148,.T.);
#5506=ORIENTED_EDGE('',*,*,#3993,.T.);
#5507=ORIENTED_EDGE('',*,*,#4126,.F.);
#5508=ORIENTED_EDGE('',*,*,#4149,.T.);
#5509=ORIENTED_EDGE('',*,*,#4150,.T.);
#5510=ORIENTED_EDGE('',*,*,#4147,.F.);
#5511=ORIENTED_EDGE('',*,*,#4124,.F.);
#5512=ORIENTED_EDGE('',*,*,#4151,.T.);
#5513=ORIENTED_EDGE('',*,*,#4152,.T.);
#5514=ORIENTED_EDGE('',*,*,#4149,.F.);
#5515=ORIENTED_EDGE('',*,*,#4121,.F.);
#5516=ORIENTED_EDGE('',*,*,#4153,.F.);
#5517=ORIENTED_EDGE('',*,*,#4154,.T.);
#5518=ORIENTED_EDGE('',*,*,#4151,.F.);
#5519=ORIENTED_EDGE('',*,*,#4145,.F.);
#5520=ORIENTED_EDGE('',*,*,#3995,.T.);
#5521=ORIENTED_EDGE('',*,*,#4155,.T.);
#5522=ORIENTED_EDGE('',*,*,#4153,.T.);
#5523=ORIENTED_EDGE('',*,*,#4136,.F.);
#5524=ORIENTED_EDGE('',*,*,#4036,.T.);
#5525=ORIENTED_EDGE('',*,*,#3949,.T.);
#5526=ORIENTED_EDGE('',*,*,#3997,.T.);
#5527=ORIENTED_EDGE('',*,*,#4133,.F.);
#5528=ORIENTED_EDGE('',*,*,#4156,.T.);
#5529=ORIENTED_EDGE('',*,*,#4047,.T.);
#5530=ORIENTED_EDGE('',*,*,#4038,.T.);
#5531=ORIENTED_EDGE('',*,*,#4131,.F.);
#5532=ORIENTED_EDGE('',*,*,#4157,.F.);
#5533=ORIENTED_EDGE('',*,*,#4048,.T.);
#5534=ORIENTED_EDGE('',*,*,#4156,.F.);
#5535=ORIENTED_EDGE('',*,*,#4128,.F.);
#5536=ORIENTED_EDGE('',*,*,#4158,.F.);
#5537=ORIENTED_EDGE('',*,*,#4159,.F.);
#5538=ORIENTED_EDGE('',*,*,#4160,.F.);
#5539=ORIENTED_EDGE('',*,*,#4049,.T.);
#5540=ORIENTED_EDGE('',*,*,#4157,.T.);
#5541=ORIENTED_EDGE('',*,*,#4144,.F.);
#5542=ORIENTED_EDGE('',*,*,#4161,.T.);
#5543=ORIENTED_EDGE('',*,*,#4162,.F.);
#5544=ORIENTED_EDGE('',*,*,#4158,.T.);
#5545=ORIENTED_EDGE('',*,*,#4142,.F.);
#5546=ORIENTED_EDGE('',*,*,#4163,.T.);
#5547=ORIENTED_EDGE('',*,*,#4164,.T.);
#5548=ORIENTED_EDGE('',*,*,#4161,.F.);
#5549=ORIENTED_EDGE('',*,*,#4139,.F.);
#5550=ORIENTED_EDGE('',*,*,#4165,.F.);
#5551=ORIENTED_EDGE('',*,*,#4166,.T.);
#5552=ORIENTED_EDGE('',*,*,#4163,.F.);
#5553=ORIENTED_EDGE('',*,*,#4143,.F.);
#5554=ORIENTED_EDGE('',*,*,#4020,.T.);
#5555=ORIENTED_EDGE('',*,*,#4167,.T.);
#5556=ORIENTED_EDGE('',*,*,#4165,.T.);
#5557=ORIENTED_EDGE('',*,*,#3962,.F.);
#5558=ORIENTED_EDGE('',*,*,#4168,.T.);
#5559=ORIENTED_EDGE('',*,*,#4169,.F.);
#5560=ORIENTED_EDGE('',*,*,#3971,.F.);
#5561=ORIENTED_EDGE('',*,*,#3978,.F.);
#5562=ORIENTED_EDGE('',*,*,#4170,.T.);
#5563=ORIENTED_EDGE('',*,*,#4171,.T.);
#5564=ORIENTED_EDGE('',*,*,#4172,.F.);
#5565=ORIENTED_EDGE('',*,*,#3976,.F.);
#5566=ORIENTED_EDGE('',*,*,#4169,.T.);
#5567=ORIENTED_EDGE('',*,*,#4173,.T.);
#5568=ORIENTED_EDGE('',*,*,#4170,.F.);
#5569=ORIENTED_EDGE('',*,*,#4173,.F.);
#5570=ORIENTED_EDGE('',*,*,#4168,.F.);
#5571=ORIENTED_EDGE('',*,*,#3961,.F.);
#5572=ORIENTED_EDGE('',*,*,#3991,.F.);
#5573=ORIENTED_EDGE('',*,*,#4174,.F.);
#5574=ORIENTED_EDGE('',*,*,#4175,.F.);
#5575=ORIENTED_EDGE('',*,*,#4171,.F.);
#5576=ORIENTED_EDGE('',*,*,#4070,.T.);
#5577=ORIENTED_EDGE('',*,*,#4176,.T.);
#5578=ORIENTED_EDGE('',*,*,#4159,.T.);
#5579=ORIENTED_EDGE('',*,*,#4162,.T.);
#5580=ORIENTED_EDGE('',*,*,#4164,.F.);
#5581=ORIENTED_EDGE('',*,*,#4166,.F.);
#5582=ORIENTED_EDGE('',*,*,#4167,.F.);
#5583=ORIENTED_EDGE('',*,*,#4019,.F.);
#5584=ORIENTED_EDGE('',*,*,#4177,.F.);
#5585=ORIENTED_EDGE('',*,*,#4054,.T.);
#5586=ORIENTED_EDGE('',*,*,#3984,.F.);
#5587=ORIENTED_EDGE('',*,*,#4178,.T.);
#5588=ORIENTED_EDGE('',*,*,#4179,.T.);
#5589=ORIENTED_EDGE('',*,*,#3987,.F.);
#5590=ORIENTED_EDGE('',*,*,#3981,.F.);
#5591=ORIENTED_EDGE('',*,*,#4180,.T.);
#5592=ORIENTED_EDGE('',*,*,#4181,.T.);
#5593=ORIENTED_EDGE('',*,*,#4178,.F.);
#5594=ORIENTED_EDGE('',*,*,#3963,.F.);
#5595=ORIENTED_EDGE('',*,*,#4182,.F.);
#5596=ORIENTED_EDGE('',*,*,#4183,.T.);
#5597=ORIENTED_EDGE('',*,*,#4180,.F.);
#5598=ORIENTED_EDGE('',*,*,#4183,.F.);
#5599=ORIENTED_EDGE('',*,*,#4184,.F.);
#5600=ORIENTED_EDGE('',*,*,#4185,.F.);
#5601=ORIENTED_EDGE('',*,*,#4015,.F.);
#5602=ORIENTED_EDGE('',*,*,#3988,.F.);
#5603=ORIENTED_EDGE('',*,*,#4179,.F.);
#5604=ORIENTED_EDGE('',*,*,#4181,.F.);
#5605=ORIENTED_EDGE('',*,*,#4060,.T.);
#5606=ORIENTED_EDGE('',*,*,#4152,.F.);
#5607=ORIENTED_EDGE('',*,*,#4154,.F.);
#5608=ORIENTED_EDGE('',*,*,#4155,.F.);
#5609=ORIENTED_EDGE('',*,*,#3994,.F.);
#5610=ORIENTED_EDGE('',*,*,#4148,.F.);
#5611=ORIENTED_EDGE('',*,*,#4150,.F.);
#5612=ORIENTED_EDGE('',*,*,#4065,.T.);
#5613=ORIENTED_EDGE('',*,*,#4176,.F.);
#5614=ORIENTED_EDGE('',*,*,#4186,.F.);
#5615=ORIENTED_EDGE('',*,*,#4050,.T.);
#5616=ORIENTED_EDGE('',*,*,#4160,.T.);
#5617=ORIENTED_EDGE('',*,*,#3923,.T.);
#5618=ORIENTED_EDGE('',*,*,#4053,.T.);
#5619=ORIENTED_EDGE('',*,*,#4187,.T.);
#5620=ORIENTED_EDGE('',*,*,#4184,.T.);
#5621=ORIENTED_EDGE('',*,*,#4182,.T.);
#5622=ORIENTED_EDGE('',*,*,#3969,.F.);
#5623=ORIENTED_EDGE('',*,*,#4172,.T.);
#5624=ORIENTED_EDGE('',*,*,#4175,.T.);
#5625=ORIENTED_EDGE('',*,*,#4188,.F.);
#5626=ORIENTED_EDGE('',*,*,#3946,.T.);
#5627=ORIENTED_EDGE('',*,*,#3937,.T.);
#5628=ORIENTED_EDGE('',*,*,#3932,.T.);
#5629=ORIENTED_EDGE('',*,*,#3929,.T.);
#5630=ORIENTED_EDGE('',*,*,#3927,.T.);
#5631=ORIENTED_EDGE('',*,*,#4177,.T.);
#5632=ORIENTED_EDGE('',*,*,#4018,.F.);
#5633=ORIENTED_EDGE('',*,*,#4051,.T.);
#5634=ORIENTED_EDGE('',*,*,#4186,.T.);
#5635=ORIENTED_EDGE('',*,*,#4185,.T.);
#5636=ORIENTED_EDGE('',*,*,#4187,.F.);
#5637=ORIENTED_EDGE('',*,*,#4052,.T.);
#5638=ORIENTED_EDGE('',*,*,#4016,.T.);
#5639=ORIENTED_EDGE('',*,*,#4174,.T.);
#5640=ORIENTED_EDGE('',*,*,#3998,.F.);
#5641=ORIENTED_EDGE('',*,*,#3947,.T.);
#5642=ORIENTED_EDGE('',*,*,#4188,.T.);
#5643=ORIENTED_EDGE('',*,*,#4189,.T.);
#5644=ORIENTED_EDGE('',*,*,#4190,.F.);
#5645=ORIENTED_EDGE('',*,*,#4191,.F.);
#5646=ORIENTED_EDGE('',*,*,#4192,.F.);
#5647=ORIENTED_EDGE('',*,*,#4193,.F.);
#5648=ORIENTED_EDGE('',*,*,#4194,.F.);
#5649=ORIENTED_EDGE('',*,*,#4195,.T.);
#5650=ORIENTED_EDGE('',*,*,#4196,.F.);
#5651=ORIENTED_EDGE('',*,*,#4197,.F.);
#5652=ORIENTED_EDGE('',*,*,#4198,.F.);
#5653=ORIENTED_EDGE('',*,*,#4199,.T.);
#5654=ORIENTED_EDGE('',*,*,#4200,.T.);
#5655=ORIENTED_EDGE('',*,*,#4201,.T.);
#5656=ORIENTED_EDGE('',*,*,#4202,.T.);
#5657=ORIENTED_EDGE('',*,*,#4203,.T.);
#5658=ORIENTED_EDGE('',*,*,#4204,.T.);
#5659=ORIENTED_EDGE('',*,*,#4205,.T.);
#5660=ORIENTED_EDGE('',*,*,#4206,.T.);
#5661=ORIENTED_EDGE('',*,*,#4207,.T.);
#5662=ORIENTED_EDGE('',*,*,#4208,.T.);
#5663=ORIENTED_EDGE('',*,*,#4209,.T.);
#5664=ORIENTED_EDGE('',*,*,#4210,.T.);
#5665=ORIENTED_EDGE('',*,*,#4211,.T.);
#5666=ORIENTED_EDGE('',*,*,#4212,.T.);
#5667=ORIENTED_EDGE('',*,*,#4213,.T.);
#5668=ORIENTED_EDGE('',*,*,#4208,.F.);
#5669=ORIENTED_EDGE('',*,*,#4214,.T.);
#5670=ORIENTED_EDGE('',*,*,#4215,.T.);
#5671=ORIENTED_EDGE('',*,*,#4216,.T.);
#5672=ORIENTED_EDGE('',*,*,#4217,.T.);
#5673=ORIENTED_EDGE('',*,*,#4218,.T.);
#5674=ORIENTED_EDGE('',*,*,#4219,.T.);
#5675=ORIENTED_EDGE('',*,*,#4217,.F.);
#5676=ORIENTED_EDGE('',*,*,#4220,.T.);
#5677=ORIENTED_EDGE('',*,*,#4221,.T.);
#5678=ORIENTED_EDGE('',*,*,#4222,.T.);
#5679=ORIENTED_EDGE('',*,*,#4223,.T.);
#5680=ORIENTED_EDGE('',*,*,#4224,.T.);
#5681=ORIENTED_EDGE('',*,*,#4221,.F.);
#5682=ORIENTED_EDGE('',*,*,#4223,.F.);
#5683=ORIENTED_EDGE('',*,*,#4225,.T.);
#5684=ORIENTED_EDGE('',*,*,#4212,.F.);
#5685=ORIENTED_EDGE('',*,*,#4226,.T.);
#5686=ORIENTED_EDGE('',*,*,#4209,.F.);
#5687=ORIENTED_EDGE('',*,*,#4227,.F.);
#5688=ORIENTED_EDGE('',*,*,#4228,.F.);
#5689=ORIENTED_EDGE('',*,*,#4229,.T.);
#5690=ORIENTED_EDGE('',*,*,#4213,.F.);
#5691=ORIENTED_EDGE('',*,*,#4230,.F.);
#5692=ORIENTED_EDGE('',*,*,#4231,.F.);
#5693=ORIENTED_EDGE('',*,*,#4227,.T.);
#5694=ORIENTED_EDGE('',*,*,#4225,.F.);
#5695=ORIENTED_EDGE('',*,*,#4232,.T.);
#5696=ORIENTED_EDGE('',*,*,#4233,.T.);
#5697=ORIENTED_EDGE('',*,*,#4234,.T.);
#5698=ORIENTED_EDGE('',*,*,#4230,.T.);
#5699=ORIENTED_EDGE('',*,*,#4222,.F.);
#5700=ORIENTED_EDGE('',*,*,#4235,.F.);
#5701=ORIENTED_EDGE('',*,*,#4236,.T.);
#5702=ORIENTED_EDGE('',*,*,#4232,.F.);
#5703=ORIENTED_EDGE('',*,*,#4237,.T.);
#5704=ORIENTED_EDGE('',*,*,#4235,.T.);
#5705=ORIENTED_EDGE('',*,*,#4220,.F.);
#5706=ORIENTED_EDGE('',*,*,#4238,.F.);
#5707=ORIENTED_EDGE('',*,*,#4239,.F.);
#5708=ORIENTED_EDGE('',*,*,#4240,.T.);
#5709=ORIENTED_EDGE('',*,*,#4241,.F.);
#5710=ORIENTED_EDGE('',*,*,#4242,.F.);
#5711=ORIENTED_EDGE('',*,*,#4210,.F.);
#5712=ORIENTED_EDGE('',*,*,#4243,.T.);
#5713=ORIENTED_EDGE('',*,*,#4215,.F.);
#5714=ORIENTED_EDGE('',*,*,#4244,.T.);
#5715=ORIENTED_EDGE('',*,*,#4216,.F.);
#5716=ORIENTED_EDGE('',*,*,#4245,.F.);
#5717=ORIENTED_EDGE('',*,*,#4246,.F.);
#5718=ORIENTED_EDGE('',*,*,#4238,.T.);
#5719=ORIENTED_EDGE('',*,*,#4211,.F.);
#5720=ORIENTED_EDGE('',*,*,#4244,.F.);
#5721=ORIENTED_EDGE('',*,*,#4218,.F.);
#5722=ORIENTED_EDGE('',*,*,#4219,.F.);
#5723=ORIENTED_EDGE('',*,*,#4224,.F.);
#5724=ORIENTED_EDGE('',*,*,#4226,.F.);
#5725=ORIENTED_EDGE('',*,*,#4214,.F.);
#5726=ORIENTED_EDGE('',*,*,#4234,.F.);
#5727=ORIENTED_EDGE('',*,*,#4247,.T.);
#5728=ORIENTED_EDGE('',*,*,#4248,.T.);
#5729=ORIENTED_EDGE('',*,*,#4249,.F.);
#5730=ORIENTED_EDGE('',*,*,#4250,.F.);
#5731=ORIENTED_EDGE('',*,*,#4190,.T.);
#5732=ORIENTED_EDGE('',*,*,#4251,.T.);
#5733=ORIENTED_EDGE('',*,*,#4252,.T.);
#5734=ORIENTED_EDGE('',*,*,#4253,.T.);
#5735=ORIENTED_EDGE('',*,*,#4254,.T.);
#5736=ORIENTED_EDGE('',*,*,#4239,.T.);
#5737=ORIENTED_EDGE('',*,*,#4246,.T.);
#5738=ORIENTED_EDGE('',*,*,#4255,.T.);
#5739=ORIENTED_EDGE('',*,*,#4228,.T.);
#5740=ORIENTED_EDGE('',*,*,#4231,.T.);
#5741=ORIENTED_EDGE('',*,*,#4256,.F.);
#5742=ORIENTED_EDGE('',*,*,#4257,.T.);
#5743=ORIENTED_EDGE('',*,*,#4237,.F.);
#5744=ORIENTED_EDGE('',*,*,#4257,.F.);
#5745=ORIENTED_EDGE('',*,*,#4243,.F.);
#5746=ORIENTED_EDGE('',*,*,#4229,.F.);
#5747=ORIENTED_EDGE('',*,*,#4255,.F.);
#5748=ORIENTED_EDGE('',*,*,#4245,.T.);
#5749=ORIENTED_EDGE('',*,*,#4256,.T.);
#5750=ORIENTED_EDGE('',*,*,#4189,.F.);
#5751=ORIENTED_EDGE('',*,*,#4258,.F.);
#5752=ORIENTED_EDGE('',*,*,#4259,.F.);
#5753=ORIENTED_EDGE('',*,*,#4251,.F.);
#5754=ORIENTED_EDGE('',*,*,#4253,.F.);
#5755=ORIENTED_EDGE('',*,*,#4260,.T.);
#5756=ORIENTED_EDGE('',*,*,#4261,.F.);
#5757=ORIENTED_EDGE('',*,*,#4262,.F.);
#5758=ORIENTED_EDGE('',*,*,#4252,.F.);
#5759=ORIENTED_EDGE('',*,*,#4259,.T.);
#5760=ORIENTED_EDGE('',*,*,#4263,.F.);
#5761=ORIENTED_EDGE('',*,*,#4264,.F.);
#5762=ORIENTED_EDGE('',*,*,#4260,.F.);
#5763=ORIENTED_EDGE('',*,*,#4254,.F.);
#5764=ORIENTED_EDGE('',*,*,#4262,.T.);
#5765=ORIENTED_EDGE('',*,*,#4265,.F.);
#5766=ORIENTED_EDGE('',*,*,#4240,.F.);
#5767=ORIENTED_EDGE('',*,*,#4242,.T.);
#5768=ORIENTED_EDGE('',*,*,#4266,.T.);
#5769=ORIENTED_EDGE('',*,*,#4267,.T.);
#5770=ORIENTED_EDGE('',*,*,#4268,.T.);
#5771=ORIENTED_EDGE('',*,*,#4269,.T.);
#5772=ORIENTED_EDGE('',*,*,#4270,.T.);
#5773=ORIENTED_EDGE('',*,*,#4271,.T.);
#5774=ORIENTED_EDGE('',*,*,#4272,.T.);
#5775=ORIENTED_EDGE('',*,*,#4273,.F.);
#5776=ORIENTED_EDGE('',*,*,#4274,.F.);
#5777=ORIENTED_EDGE('',*,*,#4275,.F.);
#5778=ORIENTED_EDGE('',*,*,#4276,.F.);
#5779=ORIENTED_EDGE('',*,*,#4247,.F.);
#5780=ORIENTED_EDGE('',*,*,#4233,.F.);
#5781=ORIENTED_EDGE('',*,*,#4236,.F.);
#5782=ORIENTED_EDGE('',*,*,#4277,.T.);
#5783=ORIENTED_EDGE('',*,*,#4278,.T.);
#5784=ORIENTED_EDGE('',*,*,#4279,.F.);
#5785=ORIENTED_EDGE('',*,*,#4280,.F.);
#5786=ORIENTED_EDGE('',*,*,#4281,.F.);
#5787=ORIENTED_EDGE('',*,*,#4282,.T.);
#5788=ORIENTED_EDGE('',*,*,#4283,.F.);
#5789=ORIENTED_EDGE('',*,*,#4282,.F.);
#5790=ORIENTED_EDGE('',*,*,#4284,.F.);
#5791=ORIENTED_EDGE('',*,*,#4272,.F.);
#5792=ORIENTED_EDGE('',*,*,#4285,.F.);
#5793=ORIENTED_EDGE('',*,*,#4199,.F.);
#5794=ORIENTED_EDGE('',*,*,#4286,.F.);
#5795=ORIENTED_EDGE('',*,*,#4287,.T.);
#5796=ORIENTED_EDGE('',*,*,#4288,.F.);
#5797=ORIENTED_EDGE('',*,*,#4287,.F.);
#5798=ORIENTED_EDGE('',*,*,#4289,.F.);
#5799=ORIENTED_EDGE('',*,*,#4290,.T.);
#5800=ORIENTED_EDGE('',*,*,#4291,.F.);
#5801=ORIENTED_EDGE('',*,*,#4290,.F.);
#5802=ORIENTED_EDGE('',*,*,#4292,.F.);
#5803=ORIENTED_EDGE('',*,*,#4280,.T.);
#5804=ORIENTED_EDGE('',*,*,#4284,.T.);
#5805=ORIENTED_EDGE('',*,*,#4281,.T.);
#5806=ORIENTED_EDGE('',*,*,#4292,.T.);
#5807=ORIENTED_EDGE('',*,*,#4289,.T.);
#5808=ORIENTED_EDGE('',*,*,#4286,.T.);
#5809=ORIENTED_EDGE('',*,*,#4198,.T.);
#5810=ORIENTED_EDGE('',*,*,#4293,.T.);
#5811=ORIENTED_EDGE('',*,*,#4294,.F.);
#5812=ORIENTED_EDGE('',*,*,#4295,.F.);
#5813=ORIENTED_EDGE('',*,*,#4273,.T.);
#5814=ORIENTED_EDGE('',*,*,#4264,.T.);
#5815=ORIENTED_EDGE('',*,*,#4296,.T.);
#5816=ORIENTED_EDGE('',*,*,#4297,.T.);
#5817=ORIENTED_EDGE('',*,*,#4298,.T.);
#5818=ORIENTED_EDGE('',*,*,#4266,.F.);
#5819=ORIENTED_EDGE('',*,*,#4241,.T.);
#5820=ORIENTED_EDGE('',*,*,#4265,.T.);
#5821=ORIENTED_EDGE('',*,*,#4261,.T.);
#5822=ORIENTED_EDGE('',*,*,#4299,.T.);
#5823=ORIENTED_EDGE('',*,*,#4300,.F.);
#5824=ORIENTED_EDGE('',*,*,#4301,.T.);
#5825=ORIENTED_EDGE('',*,*,#4302,.F.);
#5826=ORIENTED_EDGE('',*,*,#4303,.T.);
#5827=ORIENTED_EDGE('',*,*,#4304,.F.);
#5828=ORIENTED_EDGE('',*,*,#4305,.F.);
#5829=ORIENTED_EDGE('',*,*,#4306,.T.);
#5830=ORIENTED_EDGE('',*,*,#4307,.F.);
#5831=ORIENTED_EDGE('',*,*,#4308,.T.);
#5832=ORIENTED_EDGE('',*,*,#4297,.F.);
#5833=ORIENTED_EDGE('',*,*,#4309,.T.);
#5834=ORIENTED_EDGE('',*,*,#4204,.F.);
#5835=ORIENTED_EDGE('',*,*,#4310,.T.);
#5836=ORIENTED_EDGE('',*,*,#4300,.T.);
#5837=ORIENTED_EDGE('',*,*,#4311,.T.);
#5838=ORIENTED_EDGE('',*,*,#4305,.T.);
#5839=ORIENTED_EDGE('',*,*,#4312,.T.);
#5840=ORIENTED_EDGE('',*,*,#4270,.F.);
#5841=ORIENTED_EDGE('',*,*,#4313,.T.);
#5842=ORIENTED_EDGE('',*,*,#4268,.F.);
#5843=ORIENTED_EDGE('',*,*,#4314,.T.);
#5844=ORIENTED_EDGE('',*,*,#4307,.T.);
#5845=ORIENTED_EDGE('',*,*,#4315,.T.);
#5846=ORIENTED_EDGE('',*,*,#4202,.F.);
#5847=ORIENTED_EDGE('',*,*,#4316,.T.);
#5848=ORIENTED_EDGE('',*,*,#4302,.T.);
#5849=ORIENTED_EDGE('',*,*,#4283,.T.);
#5850=ORIENTED_EDGE('',*,*,#4271,.F.);
#5851=ORIENTED_EDGE('',*,*,#4312,.F.);
#5852=ORIENTED_EDGE('',*,*,#4304,.T.);
#5853=ORIENTED_EDGE('',*,*,#4317,.T.);
#5854=ORIENTED_EDGE('',*,*,#4200,.F.);
#5855=ORIENTED_EDGE('',*,*,#4285,.T.);
#5856=ORIENTED_EDGE('',*,*,#4288,.T.);
#5857=ORIENTED_EDGE('',*,*,#4291,.T.);
#5858=ORIENTED_EDGE('',*,*,#4279,.T.);
#5859=ORIENTED_EDGE('',*,*,#4301,.F.);
#5860=ORIENTED_EDGE('',*,*,#4310,.F.);
#5861=ORIENTED_EDGE('',*,*,#4203,.F.);
#5862=ORIENTED_EDGE('',*,*,#4315,.F.);
#5863=ORIENTED_EDGE('',*,*,#4298,.F.);
#5864=ORIENTED_EDGE('',*,*,#4308,.F.);
#5865=ORIENTED_EDGE('',*,*,#4314,.F.);
#5866=ORIENTED_EDGE('',*,*,#4267,.F.);
#5867=ORIENTED_EDGE('',*,*,#4313,.F.);
#5868=ORIENTED_EDGE('',*,*,#4306,.F.);
#5869=ORIENTED_EDGE('',*,*,#4311,.F.);
#5870=ORIENTED_EDGE('',*,*,#4269,.F.);
#5871=ORIENTED_EDGE('',*,*,#4258,.T.);
#5872=ORIENTED_EDGE('',*,*,#4205,.F.);
#5873=ORIENTED_EDGE('',*,*,#4309,.F.);
#5874=ORIENTED_EDGE('',*,*,#4299,.F.);
#5875=ORIENTED_EDGE('',*,*,#4296,.F.);
#5876=ORIENTED_EDGE('',*,*,#4263,.T.);
#5877=ORIENTED_EDGE('',*,*,#4201,.F.);
#5878=ORIENTED_EDGE('',*,*,#4317,.F.);
#5879=ORIENTED_EDGE('',*,*,#4303,.F.);
#5880=ORIENTED_EDGE('',*,*,#4316,.F.);
#5881=ORIENTED_EDGE('',*,*,#4206,.F.);
#5882=ORIENTED_EDGE('',*,*,#4318,.T.);
#5883=ORIENTED_EDGE('',*,*,#4319,.T.);
#5884=ORIENTED_EDGE('',*,*,#4318,.F.);
#5885=ORIENTED_EDGE('',*,*,#4319,.F.);
#5886=ORIENTED_EDGE('',*,*,#4278,.F.);
#5887=ORIENTED_EDGE('',*,*,#4320,.T.);
#5888=ORIENTED_EDGE('',*,*,#4321,.T.);
#5889=ORIENTED_EDGE('',*,*,#4320,.F.);
#5890=ORIENTED_EDGE('',*,*,#4321,.F.);
#5891=ORIENTED_EDGE('',*,*,#4277,.F.);
#5892=ORIENTED_EDGE('',*,*,#4322,.T.);
#5893=ORIENTED_EDGE('',*,*,#4323,.T.);
#5894=ORIENTED_EDGE('',*,*,#4322,.F.);
#5895=ORIENTED_EDGE('',*,*,#4323,.F.);
#5896=ORIENTED_EDGE('',*,*,#4207,.F.);
#5897=ORIENTED_EDGE('',*,*,#4324,.T.);
#5898=ORIENTED_EDGE('',*,*,#4325,.T.);
#5899=ORIENTED_EDGE('',*,*,#4324,.F.);
#5900=ORIENTED_EDGE('',*,*,#4325,.F.);
#5901=ORIENTED_EDGE('',*,*,#4326,.T.);
#5902=ORIENTED_EDGE('',*,*,#4327,.T.);
#5903=ORIENTED_EDGE('',*,*,#4328,.T.);
#5904=ORIENTED_EDGE('',*,*,#4329,.T.);
#5905=ORIENTED_EDGE('',*,*,#4330,.T.);
#5906=ORIENTED_EDGE('',*,*,#4331,.T.);
#5907=ORIENTED_EDGE('',*,*,#4328,.F.);
#5908=ORIENTED_EDGE('',*,*,#4332,.T.);
#5909=ORIENTED_EDGE('',*,*,#4333,.T.);
#5910=ORIENTED_EDGE('',*,*,#4334,.T.);
#5911=ORIENTED_EDGE('',*,*,#4330,.F.);
#5912=ORIENTED_EDGE('',*,*,#4335,.T.);
#5913=ORIENTED_EDGE('',*,*,#4336,.T.);
#5914=ORIENTED_EDGE('',*,*,#4337,.T.);
#5915=ORIENTED_EDGE('',*,*,#4333,.F.);
#5916=ORIENTED_EDGE('',*,*,#4338,.T.);
#5917=ORIENTED_EDGE('',*,*,#4339,.T.);
#5918=ORIENTED_EDGE('',*,*,#4340,.T.);
#5919=ORIENTED_EDGE('',*,*,#4336,.F.);
#5920=ORIENTED_EDGE('',*,*,#4341,.T.);
#5921=ORIENTED_EDGE('',*,*,#4342,.T.);
#5922=ORIENTED_EDGE('',*,*,#4343,.T.);
#5923=ORIENTED_EDGE('',*,*,#4339,.F.);
#5924=ORIENTED_EDGE('',*,*,#4344,.T.);
#5925=ORIENTED_EDGE('',*,*,#4345,.T.);
#5926=ORIENTED_EDGE('',*,*,#4346,.T.);
#5927=ORIENTED_EDGE('',*,*,#4342,.F.);
#5928=ORIENTED_EDGE('',*,*,#4249,.T.);
#5929=ORIENTED_EDGE('',*,*,#4347,.T.);
#5930=ORIENTED_EDGE('',*,*,#4348,.T.);
#5931=ORIENTED_EDGE('',*,*,#4345,.F.);
#5932=ORIENTED_EDGE('',*,*,#4349,.T.);
#5933=ORIENTED_EDGE('',*,*,#4350,.T.);
#5934=ORIENTED_EDGE('',*,*,#4351,.T.);
#5935=ORIENTED_EDGE('',*,*,#4347,.F.);
#5936=ORIENTED_EDGE('',*,*,#4352,.T.);
#5937=ORIENTED_EDGE('',*,*,#4353,.T.);
#5938=ORIENTED_EDGE('',*,*,#4354,.T.);
#5939=ORIENTED_EDGE('',*,*,#4350,.F.);
#5940=ORIENTED_EDGE('',*,*,#4355,.T.);
#5941=ORIENTED_EDGE('',*,*,#4356,.T.);
#5942=ORIENTED_EDGE('',*,*,#4357,.T.);
#5943=ORIENTED_EDGE('',*,*,#4353,.F.);
#5944=ORIENTED_EDGE('',*,*,#4294,.T.);
#5945=ORIENTED_EDGE('',*,*,#4326,.F.);
#5946=ORIENTED_EDGE('',*,*,#4358,.T.);
#5947=ORIENTED_EDGE('',*,*,#4356,.F.);
#5948=ORIENTED_EDGE('',*,*,#4359,.T.);
#5949=ORIENTED_EDGE('',*,*,#4344,.F.);
#5950=ORIENTED_EDGE('',*,*,#4360,.F.);
#5951=ORIENTED_EDGE('',*,*,#4191,.T.);
#5952=ORIENTED_EDGE('',*,*,#4250,.T.);
#5953=ORIENTED_EDGE('',*,*,#4341,.F.);
#5954=ORIENTED_EDGE('',*,*,#4361,.F.);
#5955=ORIENTED_EDGE('',*,*,#4192,.T.);
#5956=ORIENTED_EDGE('',*,*,#4360,.T.);
#5957=ORIENTED_EDGE('',*,*,#4338,.F.);
#5958=ORIENTED_EDGE('',*,*,#4362,.F.);
#5959=ORIENTED_EDGE('',*,*,#4193,.T.);
#5960=ORIENTED_EDGE('',*,*,#4361,.T.);
#5961=ORIENTED_EDGE('',*,*,#4335,.F.);
#5962=ORIENTED_EDGE('',*,*,#4363,.F.);
#5963=ORIENTED_EDGE('',*,*,#4194,.T.);
#5964=ORIENTED_EDGE('',*,*,#4362,.T.);
#5965=ORIENTED_EDGE('',*,*,#4332,.F.);
#5966=ORIENTED_EDGE('',*,*,#4364,.F.);
#5967=ORIENTED_EDGE('',*,*,#4195,.F.);
#5968=ORIENTED_EDGE('',*,*,#4363,.T.);
#5969=ORIENTED_EDGE('',*,*,#4327,.F.);
#5970=ORIENTED_EDGE('',*,*,#4365,.F.);
#5971=ORIENTED_EDGE('',*,*,#4196,.T.);
#5972=ORIENTED_EDGE('',*,*,#4364,.T.);
#5973=ORIENTED_EDGE('',*,*,#4329,.F.);
#5974=ORIENTED_EDGE('',*,*,#4331,.F.);
#5975=ORIENTED_EDGE('',*,*,#4334,.F.);
#5976=ORIENTED_EDGE('',*,*,#4337,.F.);
#5977=ORIENTED_EDGE('',*,*,#4340,.F.);
#5978=ORIENTED_EDGE('',*,*,#4343,.F.);
#5979=ORIENTED_EDGE('',*,*,#4346,.F.);
#5980=ORIENTED_EDGE('',*,*,#4348,.F.);
#5981=ORIENTED_EDGE('',*,*,#4351,.F.);
#5982=ORIENTED_EDGE('',*,*,#4354,.F.);
#5983=ORIENTED_EDGE('',*,*,#4357,.F.);
#5984=ORIENTED_EDGE('',*,*,#4358,.F.);
#5985=ORIENTED_EDGE('',*,*,#4359,.F.);
#5986=ORIENTED_EDGE('',*,*,#4293,.F.);
#5987=ORIENTED_EDGE('',*,*,#4197,.T.);
#5988=ORIENTED_EDGE('',*,*,#4365,.T.);
#5989=ORIENTED_EDGE('',*,*,#4355,.F.);
#5990=ORIENTED_EDGE('',*,*,#4366,.F.);
#5991=ORIENTED_EDGE('',*,*,#4274,.T.);
#5992=ORIENTED_EDGE('',*,*,#4295,.T.);
#5993=ORIENTED_EDGE('',*,*,#4352,.F.);
#5994=ORIENTED_EDGE('',*,*,#4367,.F.);
#5995=ORIENTED_EDGE('',*,*,#4275,.T.);
#5996=ORIENTED_EDGE('',*,*,#4366,.T.);
#5997=ORIENTED_EDGE('',*,*,#4349,.F.);
#5998=ORIENTED_EDGE('',*,*,#4248,.F.);
#5999=ORIENTED_EDGE('',*,*,#4276,.T.);
#6000=ORIENTED_EDGE('',*,*,#4367,.T.);
#6001=ORIENTED_EDGE('',*,*,#4368,.F.);
#6002=ORIENTED_EDGE('',*,*,#4369,.T.);
#6003=ORIENTED_EDGE('',*,*,#4370,.F.);
#6004=ORIENTED_EDGE('',*,*,#4369,.F.);
#6005=ORIENTED_EDGE('',*,*,#4371,.F.);
#6006=ORIENTED_EDGE('',*,*,#4372,.T.);
#6007=ORIENTED_EDGE('',*,*,#4373,.F.);
#6008=ORIENTED_EDGE('',*,*,#4372,.F.);
#6009=ORIENTED_EDGE('',*,*,#4374,.F.);
#6010=ORIENTED_EDGE('',*,*,#4375,.T.);
#6011=ORIENTED_EDGE('',*,*,#4376,.F.);
#6012=ORIENTED_EDGE('',*,*,#4375,.F.);
#6013=ORIENTED_EDGE('',*,*,#4377,.F.);
#6014=ORIENTED_EDGE('',*,*,#4378,.T.);
#6015=ORIENTED_EDGE('',*,*,#4379,.F.);
#6016=ORIENTED_EDGE('',*,*,#4378,.F.);
#6017=ORIENTED_EDGE('',*,*,#4380,.T.);
#6018=ORIENTED_EDGE('',*,*,#4381,.T.);
#6019=ORIENTED_EDGE('',*,*,#4382,.T.);
#6020=ORIENTED_EDGE('',*,*,#4383,.T.);
#6021=ORIENTED_EDGE('',*,*,#4384,.T.);
#6022=ORIENTED_EDGE('',*,*,#4385,.T.);
#6023=ORIENTED_EDGE('',*,*,#4386,.T.);
#6024=ORIENTED_EDGE('',*,*,#4387,.T.);
#6025=ORIENTED_EDGE('',*,*,#4388,.T.);
#6026=ORIENTED_EDGE('',*,*,#4389,.T.);
#6027=ORIENTED_EDGE('',*,*,#4390,.T.);
#6028=ORIENTED_EDGE('',*,*,#4391,.T.);
#6029=ORIENTED_EDGE('',*,*,#4392,.T.);
#6030=ORIENTED_EDGE('',*,*,#4393,.T.);
#6031=ORIENTED_EDGE('',*,*,#4394,.T.);
#6032=ORIENTED_EDGE('',*,*,#4395,.T.);
#6033=ORIENTED_EDGE('',*,*,#4396,.F.);
#6034=ORIENTED_EDGE('',*,*,#4397,.F.);
#6035=ORIENTED_EDGE('',*,*,#4398,.F.);
#6036=ORIENTED_EDGE('',*,*,#4389,.F.);
#6037=ORIENTED_EDGE('',*,*,#4398,.T.);
#6038=ORIENTED_EDGE('',*,*,#4399,.F.);
#6039=ORIENTED_EDGE('',*,*,#4400,.F.);
#6040=ORIENTED_EDGE('',*,*,#4390,.F.);
#6041=ORIENTED_EDGE('',*,*,#4400,.T.);
#6042=ORIENTED_EDGE('',*,*,#4401,.F.);
#6043=ORIENTED_EDGE('',*,*,#4402,.F.);
#6044=ORIENTED_EDGE('',*,*,#4391,.F.);
#6045=ORIENTED_EDGE('',*,*,#4373,.T.);
#6046=ORIENTED_EDGE('',*,*,#4379,.T.);
#6047=ORIENTED_EDGE('',*,*,#4402,.T.);
#6048=ORIENTED_EDGE('',*,*,#4403,.F.);
#6049=ORIENTED_EDGE('',*,*,#4404,.F.);
#6050=ORIENTED_EDGE('',*,*,#4392,.F.);
#6051=ORIENTED_EDGE('',*,*,#4404,.T.);
#6052=ORIENTED_EDGE('',*,*,#4405,.F.);
#6053=ORIENTED_EDGE('',*,*,#4406,.F.);
#6054=ORIENTED_EDGE('',*,*,#4393,.F.);
#6055=ORIENTED_EDGE('',*,*,#4406,.T.);
#6056=ORIENTED_EDGE('',*,*,#4407,.F.);
#6057=ORIENTED_EDGE('',*,*,#4408,.F.);
#6058=ORIENTED_EDGE('',*,*,#4394,.F.);
#6059=ORIENTED_EDGE('',*,*,#4408,.T.);
#6060=ORIENTED_EDGE('',*,*,#4409,.F.);
#6061=ORIENTED_EDGE('',*,*,#4410,.F.);
#6062=ORIENTED_EDGE('',*,*,#4395,.F.);
#6063=ORIENTED_EDGE('',*,*,#4368,.T.);
#6064=ORIENTED_EDGE('',*,*,#4374,.T.);
#6065=ORIENTED_EDGE('',*,*,#4410,.T.);
#6066=ORIENTED_EDGE('',*,*,#4411,.F.);
#6067=ORIENTED_EDGE('',*,*,#4396,.T.);
#6068=ORIENTED_EDGE('',*,*,#4388,.F.);
#6069=ORIENTED_EDGE('',*,*,#4412,.F.);
#6070=ORIENTED_EDGE('',*,*,#4413,.F.);
#6071=ORIENTED_EDGE('',*,*,#4414,.F.);
#6072=ORIENTED_EDGE('',*,*,#4381,.F.);
#6073=ORIENTED_EDGE('',*,*,#4414,.T.);
#6074=ORIENTED_EDGE('',*,*,#4415,.F.);
#6075=ORIENTED_EDGE('',*,*,#4416,.F.);
#6076=ORIENTED_EDGE('',*,*,#4382,.F.);
#6077=ORIENTED_EDGE('',*,*,#4416,.T.);
#6078=ORIENTED_EDGE('',*,*,#4417,.F.);
#6079=ORIENTED_EDGE('',*,*,#4418,.F.);
#6080=ORIENTED_EDGE('',*,*,#4383,.F.);
#6081=ORIENTED_EDGE('',*,*,#4370,.T.);
#6082=ORIENTED_EDGE('',*,*,#4376,.T.);
#6083=ORIENTED_EDGE('',*,*,#4418,.T.);
#6084=ORIENTED_EDGE('',*,*,#4419,.F.);
#6085=ORIENTED_EDGE('',*,*,#4420,.F.);
#6086=ORIENTED_EDGE('',*,*,#4384,.F.);
#6087=ORIENTED_EDGE('',*,*,#4420,.T.);
#6088=ORIENTED_EDGE('',*,*,#4421,.F.);
#6089=ORIENTED_EDGE('',*,*,#4422,.F.);
#6090=ORIENTED_EDGE('',*,*,#4385,.F.);
#6091=ORIENTED_EDGE('',*,*,#4422,.T.);
#6092=ORIENTED_EDGE('',*,*,#4423,.F.);
#6093=ORIENTED_EDGE('',*,*,#4424,.F.);
#6094=ORIENTED_EDGE('',*,*,#4386,.F.);
#6095=ORIENTED_EDGE('',*,*,#4424,.T.);
#6096=ORIENTED_EDGE('',*,*,#4425,.F.);
#6097=ORIENTED_EDGE('',*,*,#4426,.F.);
#6098=ORIENTED_EDGE('',*,*,#4387,.F.);
#6099=ORIENTED_EDGE('',*,*,#4371,.T.);
#6100=ORIENTED_EDGE('',*,*,#4377,.T.);
#6101=ORIENTED_EDGE('',*,*,#4426,.T.);
#6102=ORIENTED_EDGE('',*,*,#4427,.F.);
#6103=ORIENTED_EDGE('',*,*,#4412,.T.);
#6104=ORIENTED_EDGE('',*,*,#4380,.F.);
#6105=ORIENTED_EDGE('',*,*,#4427,.T.);
#6106=ORIENTED_EDGE('',*,*,#4425,.T.);
#6107=ORIENTED_EDGE('',*,*,#4423,.T.);
#6108=ORIENTED_EDGE('',*,*,#4421,.T.);
#6109=ORIENTED_EDGE('',*,*,#4419,.T.);
#6110=ORIENTED_EDGE('',*,*,#4417,.T.);
#6111=ORIENTED_EDGE('',*,*,#4415,.T.);
#6112=ORIENTED_EDGE('',*,*,#4413,.T.);
#6113=ORIENTED_EDGE('',*,*,#4411,.T.);
#6114=ORIENTED_EDGE('',*,*,#4409,.T.);
#6115=ORIENTED_EDGE('',*,*,#4407,.T.);
#6116=ORIENTED_EDGE('',*,*,#4405,.T.);
#6117=ORIENTED_EDGE('',*,*,#4403,.T.);
#6118=ORIENTED_EDGE('',*,*,#4401,.T.);
#6119=ORIENTED_EDGE('',*,*,#4399,.T.);
#6120=ORIENTED_EDGE('',*,*,#4397,.T.);
#6121=ORIENTED_EDGE('',*,*,#4428,.T.);
#6122=ORIENTED_EDGE('',*,*,#4429,.T.);
#6123=ORIENTED_EDGE('',*,*,#4430,.T.);
#6124=ORIENTED_EDGE('',*,*,#4431,.T.);
#6125=ORIENTED_EDGE('',*,*,#4432,.T.);
#6126=ORIENTED_EDGE('',*,*,#4433,.T.);
#6127=ORIENTED_EDGE('',*,*,#4434,.T.);
#6128=ORIENTED_EDGE('',*,*,#4435,.T.);
#6129=ORIENTED_EDGE('',*,*,#4432,.F.);
#6130=ORIENTED_EDGE('',*,*,#4430,.F.);
#6131=ORIENTED_EDGE('',*,*,#4436,.T.);
#6132=ORIENTED_EDGE('',*,*,#4437,.T.);
#6133=ORIENTED_EDGE('',*,*,#4438,.T.);
#6134=ORIENTED_EDGE('',*,*,#4439,.T.);
#6135=ORIENTED_EDGE('',*,*,#4440,.T.);
#6136=ORIENTED_EDGE('',*,*,#4437,.F.);
#6137=ORIENTED_EDGE('',*,*,#4434,.F.);
#6138=ORIENTED_EDGE('',*,*,#4441,.T.);
#6139=ORIENTED_EDGE('',*,*,#4442,.T.);
#6140=ORIENTED_EDGE('',*,*,#4443,.T.);
#6141=ORIENTED_EDGE('',*,*,#4444,.T.);
#6142=ORIENTED_EDGE('',*,*,#4445,.T.);
#6143=ORIENTED_EDGE('',*,*,#4442,.F.);
#6144=ORIENTED_EDGE('',*,*,#4439,.F.);
#6145=ORIENTED_EDGE('',*,*,#4446,.T.);
#6146=ORIENTED_EDGE('',*,*,#4428,.F.);
#6147=ORIENTED_EDGE('',*,*,#4444,.F.);
#6148=ORIENTED_EDGE('',*,*,#4447,.T.);
#6149=ORIENTED_EDGE('',*,*,#4436,.F.);
#6150=ORIENTED_EDGE('',*,*,#4448,.F.);
#6151=ORIENTED_EDGE('',*,*,#4449,.T.);
#6152=ORIENTED_EDGE('',*,*,#4450,.T.);
#6153=ORIENTED_EDGE('',*,*,#4429,.F.);
#6154=ORIENTED_EDGE('',*,*,#4451,.F.);
#6155=ORIENTED_EDGE('',*,*,#4452,.T.);
#6156=ORIENTED_EDGE('',*,*,#4448,.T.);
#6157=ORIENTED_EDGE('',*,*,#4447,.F.);
#6158=ORIENTED_EDGE('',*,*,#4453,.F.);
#6159=ORIENTED_EDGE('',*,*,#4454,.T.);
#6160=ORIENTED_EDGE('',*,*,#4451,.T.);
#6161=ORIENTED_EDGE('',*,*,#4443,.F.);
#6162=ORIENTED_EDGE('',*,*,#4455,.F.);
#6163=ORIENTED_EDGE('',*,*,#4456,.T.);
#6164=ORIENTED_EDGE('',*,*,#4453,.T.);
#6165=ORIENTED_EDGE('',*,*,#4431,.F.);
#6166=ORIENTED_EDGE('',*,*,#4435,.F.);
#6167=ORIENTED_EDGE('',*,*,#4440,.F.);
#6168=ORIENTED_EDGE('',*,*,#4445,.F.);
#6169=ORIENTED_EDGE('',*,*,#4457,.T.);
#6170=ORIENTED_EDGE('',*,*,#4458,.T.);
#6171=ORIENTED_EDGE('',*,*,#4459,.T.);
#6172=ORIENTED_EDGE('',*,*,#4460,.T.);
#6173=ORIENTED_EDGE('',*,*,#4461,.T.);
#6174=ORIENTED_EDGE('',*,*,#4462,.T.);
#6175=ORIENTED_EDGE('',*,*,#4458,.F.);
#6176=ORIENTED_EDGE('',*,*,#4463,.T.);
#6177=ORIENTED_EDGE('',*,*,#4464,.T.);
#6178=ORIENTED_EDGE('',*,*,#4465,.T.);
#6179=ORIENTED_EDGE('',*,*,#4461,.F.);
#6180=ORIENTED_EDGE('',*,*,#4466,.T.);
#6181=ORIENTED_EDGE('',*,*,#4467,.T.);
#6182=ORIENTED_EDGE('',*,*,#4468,.T.);
#6183=ORIENTED_EDGE('',*,*,#4464,.F.);
#6184=ORIENTED_EDGE('',*,*,#4469,.T.);
#6185=ORIENTED_EDGE('',*,*,#4470,.T.);
#6186=ORIENTED_EDGE('',*,*,#4471,.T.);
#6187=ORIENTED_EDGE('',*,*,#4467,.F.);
#6188=ORIENTED_EDGE('',*,*,#4472,.T.);
#6189=ORIENTED_EDGE('',*,*,#4473,.T.);
#6190=ORIENTED_EDGE('',*,*,#4474,.T.);
#6191=ORIENTED_EDGE('',*,*,#4470,.F.);
#6192=ORIENTED_EDGE('',*,*,#4475,.T.);
#6193=ORIENTED_EDGE('',*,*,#4473,.F.);
#6194=ORIENTED_EDGE('',*,*,#4476,.T.);
#6195=ORIENTED_EDGE('',*,*,#4477,.T.);
#6196=ORIENTED_EDGE('',*,*,#4475,.F.);
#6197=ORIENTED_EDGE('',*,*,#4478,.T.);
#6198=ORIENTED_EDGE('',*,*,#4479,.F.);
#6199=ORIENTED_EDGE('',*,*,#4480,.F.);
#6200=ORIENTED_EDGE('',*,*,#4472,.F.);
#6201=ORIENTED_EDGE('',*,*,#4481,.F.);
#6202=ORIENTED_EDGE('',*,*,#4482,.F.);
#6203=ORIENTED_EDGE('',*,*,#4478,.F.);
#6204=ORIENTED_EDGE('',*,*,#4469,.F.);
#6205=ORIENTED_EDGE('',*,*,#4483,.T.);
#6206=ORIENTED_EDGE('',*,*,#4484,.F.);
#6207=ORIENTED_EDGE('',*,*,#4485,.T.);
#6208=ORIENTED_EDGE('',*,*,#4486,.F.);
#6209=ORIENTED_EDGE('',*,*,#4481,.T.);
#6210=ORIENTED_EDGE('',*,*,#4466,.F.);
#6211=ORIENTED_EDGE('',*,*,#4487,.F.);
#6212=ORIENTED_EDGE('',*,*,#4488,.F.);
#6213=ORIENTED_EDGE('',*,*,#4483,.F.);
#6214=ORIENTED_EDGE('',*,*,#4463,.F.);
#6215=ORIENTED_EDGE('',*,*,#4489,.F.);
#6216=ORIENTED_EDGE('',*,*,#4490,.F.);
#6217=ORIENTED_EDGE('',*,*,#4487,.T.);
#6218=ORIENTED_EDGE('',*,*,#4460,.F.);
#6219=ORIENTED_EDGE('',*,*,#4491,.T.);
#6220=ORIENTED_EDGE('',*,*,#4492,.F.);
#6221=ORIENTED_EDGE('',*,*,#4489,.T.);
#6222=ORIENTED_EDGE('',*,*,#4459,.F.);
#6223=ORIENTED_EDGE('',*,*,#4493,.T.);
#6224=ORIENTED_EDGE('',*,*,#4494,.T.);
#6225=ORIENTED_EDGE('',*,*,#4495,.F.);
#6226=ORIENTED_EDGE('',*,*,#4496,.T.);
#6227=ORIENTED_EDGE('',*,*,#4497,.T.);
#6228=ORIENTED_EDGE('',*,*,#4498,.T.);
#6229=ORIENTED_EDGE('',*,*,#4499,.T.);
#6230=ORIENTED_EDGE('',*,*,#4500,.T.);
#6231=ORIENTED_EDGE('',*,*,#4501,.T.);
#6232=ORIENTED_EDGE('',*,*,#4497,.F.);
#6233=ORIENTED_EDGE('',*,*,#4502,.T.);
#6234=ORIENTED_EDGE('',*,*,#4503,.T.);
#6235=ORIENTED_EDGE('',*,*,#4504,.T.);
#6236=ORIENTED_EDGE('',*,*,#4500,.F.);
#6237=ORIENTED_EDGE('',*,*,#4505,.T.);
#6238=ORIENTED_EDGE('',*,*,#4506,.T.);
#6239=ORIENTED_EDGE('',*,*,#4507,.T.);
#6240=ORIENTED_EDGE('',*,*,#4503,.F.);
#6241=ORIENTED_EDGE('',*,*,#4508,.T.);
#6242=ORIENTED_EDGE('',*,*,#4509,.T.);
#6243=ORIENTED_EDGE('',*,*,#4510,.T.);
#6244=ORIENTED_EDGE('',*,*,#4506,.F.);
#6245=ORIENTED_EDGE('',*,*,#4511,.T.);
#6246=ORIENTED_EDGE('',*,*,#4512,.T.);
#6247=ORIENTED_EDGE('',*,*,#4513,.T.);
#6248=ORIENTED_EDGE('',*,*,#4509,.F.);
#6249=ORIENTED_EDGE('',*,*,#4514,.T.);
#6250=ORIENTED_EDGE('',*,*,#4512,.F.);
#6251=ORIENTED_EDGE('',*,*,#4515,.T.);
#6252=ORIENTED_EDGE('',*,*,#4495,.T.);
#6253=ORIENTED_EDGE('',*,*,#4514,.F.);
#6254=ORIENTED_EDGE('',*,*,#4516,.F.);
#6255=ORIENTED_EDGE('',*,*,#4517,.F.);
#6256=ORIENTED_EDGE('',*,*,#4518,.F.);
#6257=ORIENTED_EDGE('',*,*,#4511,.F.);
#6258=ORIENTED_EDGE('',*,*,#4519,.F.);
#6259=ORIENTED_EDGE('',*,*,#4520,.F.);
#6260=ORIENTED_EDGE('',*,*,#4516,.T.);
#6261=ORIENTED_EDGE('',*,*,#4508,.F.);
#6262=ORIENTED_EDGE('',*,*,#4521,.T.);
#6263=ORIENTED_EDGE('',*,*,#4522,.F.);
#6264=ORIENTED_EDGE('',*,*,#4523,.F.);
#6265=ORIENTED_EDGE('',*,*,#4524,.F.);
#6266=ORIENTED_EDGE('',*,*,#4519,.T.);
#6267=ORIENTED_EDGE('',*,*,#4505,.F.);
#6268=ORIENTED_EDGE('',*,*,#4525,.T.);
#6269=ORIENTED_EDGE('',*,*,#4526,.F.);
#6270=ORIENTED_EDGE('',*,*,#4521,.F.);
#6271=ORIENTED_EDGE('',*,*,#4502,.F.);
#6272=ORIENTED_EDGE('',*,*,#4527,.F.);
#6273=ORIENTED_EDGE('',*,*,#4528,.F.);
#6274=ORIENTED_EDGE('',*,*,#4525,.F.);
#6275=ORIENTED_EDGE('',*,*,#4499,.F.);
#6276=ORIENTED_EDGE('',*,*,#4529,.T.);
#6277=ORIENTED_EDGE('',*,*,#4530,.F.);
#6278=ORIENTED_EDGE('',*,*,#4527,.T.);
#6279=ORIENTED_EDGE('',*,*,#4477,.F.);
#6280=ORIENTED_EDGE('',*,*,#4531,.T.);
#6281=ORIENTED_EDGE('',*,*,#4498,.F.);
#6282=ORIENTED_EDGE('',*,*,#4532,.T.);
#6283=ORIENTED_EDGE('',*,*,#4476,.F.);
#6284=ORIENTED_EDGE('',*,*,#4480,.T.);
#6285=ORIENTED_EDGE('',*,*,#4533,.T.);
#6286=ORIENTED_EDGE('',*,*,#4534,.T.);
#6287=ORIENTED_EDGE('',*,*,#4535,.T.);
#6288=ORIENTED_EDGE('',*,*,#4536,.T.);
#6289=ORIENTED_EDGE('',*,*,#4533,.F.);
#6290=ORIENTED_EDGE('',*,*,#4537,.T.);
#6291=ORIENTED_EDGE('',*,*,#4538,.T.);
#6292=ORIENTED_EDGE('',*,*,#4539,.T.);
#6293=ORIENTED_EDGE('',*,*,#4535,.F.);
#6294=ORIENTED_EDGE('',*,*,#4540,.T.);
#6295=ORIENTED_EDGE('',*,*,#4530,.T.);
#6296=ORIENTED_EDGE('',*,*,#4541,.T.);
#6297=ORIENTED_EDGE('',*,*,#4538,.F.);
#6298=ORIENTED_EDGE('',*,*,#4542,.T.);
#6299=ORIENTED_EDGE('',*,*,#4537,.F.);
#6300=ORIENTED_EDGE('',*,*,#4479,.T.);
#6301=ORIENTED_EDGE('',*,*,#4543,.T.);
#6302=ORIENTED_EDGE('',*,*,#4544,.T.);
#6303=ORIENTED_EDGE('',*,*,#4457,.F.);
#6304=ORIENTED_EDGE('',*,*,#4545,.T.);
#6305=ORIENTED_EDGE('',*,*,#4493,.F.);
#6306=ORIENTED_EDGE('',*,*,#4462,.F.);
#6307=ORIENTED_EDGE('',*,*,#4465,.F.);
#6308=ORIENTED_EDGE('',*,*,#4468,.F.);
#6309=ORIENTED_EDGE('',*,*,#4471,.F.);
#6310=ORIENTED_EDGE('',*,*,#4474,.F.);
#6311=ORIENTED_EDGE('',*,*,#4532,.F.);
#6312=ORIENTED_EDGE('',*,*,#4501,.F.);
#6313=ORIENTED_EDGE('',*,*,#4504,.F.);
#6314=ORIENTED_EDGE('',*,*,#4507,.F.);
#6315=ORIENTED_EDGE('',*,*,#4510,.F.);
#6316=ORIENTED_EDGE('',*,*,#4513,.F.);
#6317=ORIENTED_EDGE('',*,*,#4494,.F.);
#6318=ORIENTED_EDGE('',*,*,#4545,.F.);
#6319=ORIENTED_EDGE('',*,*,#4531,.F.);
#6320=ORIENTED_EDGE('',*,*,#4534,.F.);
#6321=ORIENTED_EDGE('',*,*,#4536,.F.);
#6322=ORIENTED_EDGE('',*,*,#4539,.F.);
#6323=ORIENTED_EDGE('',*,*,#4541,.F.);
#6324=ORIENTED_EDGE('',*,*,#4529,.F.);
#6325=ORIENTED_EDGE('',*,*,#4515,.F.);
#6326=ORIENTED_EDGE('',*,*,#4518,.T.);
#6327=ORIENTED_EDGE('',*,*,#4546,.T.);
#6328=ORIENTED_EDGE('',*,*,#4547,.T.);
#6329=ORIENTED_EDGE('',*,*,#4548,.T.);
#6330=ORIENTED_EDGE('',*,*,#4549,.T.);
#6331=ORIENTED_EDGE('',*,*,#4546,.F.);
#6332=ORIENTED_EDGE('',*,*,#4550,.T.);
#6333=ORIENTED_EDGE('',*,*,#4551,.T.);
#6334=ORIENTED_EDGE('',*,*,#4552,.T.);
#6335=ORIENTED_EDGE('',*,*,#4548,.F.);
#6336=ORIENTED_EDGE('',*,*,#4553,.T.);
#6337=ORIENTED_EDGE('',*,*,#4492,.T.);
#6338=ORIENTED_EDGE('',*,*,#4554,.T.);
#6339=ORIENTED_EDGE('',*,*,#4551,.F.);
#6340=ORIENTED_EDGE('',*,*,#4555,.T.);
#6341=ORIENTED_EDGE('',*,*,#4550,.F.);
#6342=ORIENTED_EDGE('',*,*,#4517,.T.);
#6343=ORIENTED_EDGE('',*,*,#4556,.T.);
#6344=ORIENTED_EDGE('',*,*,#4557,.T.);
#6345=ORIENTED_EDGE('',*,*,#4496,.F.);
#6346=ORIENTED_EDGE('',*,*,#4547,.F.);
#6347=ORIENTED_EDGE('',*,*,#4549,.F.);
#6348=ORIENTED_EDGE('',*,*,#4552,.F.);
#6349=ORIENTED_EDGE('',*,*,#4554,.F.);
#6350=ORIENTED_EDGE('',*,*,#4491,.F.);
#6351=ORIENTED_EDGE('',*,*,#4558,.T.);
#6352=ORIENTED_EDGE('',*,*,#4522,.T.);
#6353=ORIENTED_EDGE('',*,*,#4559,.T.);
#6354=ORIENTED_EDGE('',*,*,#4560,.T.);
#6355=ORIENTED_EDGE('',*,*,#4561,.T.);
#6356=ORIENTED_EDGE('',*,*,#4562,.T.);
#6357=ORIENTED_EDGE('',*,*,#4559,.F.);
#6358=ORIENTED_EDGE('',*,*,#4526,.T.);
#6359=ORIENTED_EDGE('',*,*,#4542,.F.);
#6360=ORIENTED_EDGE('',*,*,#4563,.T.);
#6361=ORIENTED_EDGE('',*,*,#4561,.F.);
#6362=ORIENTED_EDGE('',*,*,#4528,.T.);
#6363=ORIENTED_EDGE('',*,*,#4564,.T.);
#6364=ORIENTED_EDGE('',*,*,#4565,.T.);
#6365=ORIENTED_EDGE('',*,*,#4558,.F.);
#6366=ORIENTED_EDGE('',*,*,#4566,.T.);
#6367=ORIENTED_EDGE('',*,*,#4540,.F.);
#6368=ORIENTED_EDGE('',*,*,#4544,.F.);
#6369=ORIENTED_EDGE('',*,*,#4567,.F.);
#6370=ORIENTED_EDGE('',*,*,#4568,.F.);
#6371=ORIENTED_EDGE('',*,*,#4569,.F.);
#6372=ORIENTED_EDGE('',*,*,#4570,.F.);
#6373=ORIENTED_EDGE('',*,*,#4571,.F.);
#6374=ORIENTED_EDGE('',*,*,#4572,.T.);
#6375=ORIENTED_EDGE('',*,*,#4566,.F.);
#6376=ORIENTED_EDGE('',*,*,#4560,.F.);
#6377=ORIENTED_EDGE('',*,*,#4562,.F.);
#6378=ORIENTED_EDGE('',*,*,#4563,.F.);
#6379=ORIENTED_EDGE('',*,*,#4573,.T.);
#6380=ORIENTED_EDGE('',*,*,#4574,.T.);
#6381=ORIENTED_EDGE('',*,*,#4575,.T.);
#6382=ORIENTED_EDGE('',*,*,#4567,.T.);
#6383=ORIENTED_EDGE('',*,*,#4543,.F.);
#6384=ORIENTED_EDGE('',*,*,#4482,.T.);
#6385=ORIENTED_EDGE('',*,*,#4576,.T.);
#6386=ORIENTED_EDGE('',*,*,#4568,.T.);
#6387=ORIENTED_EDGE('',*,*,#4575,.F.);
#6388=ORIENTED_EDGE('',*,*,#4486,.T.);
#6389=ORIENTED_EDGE('',*,*,#4577,.T.);
#6390=ORIENTED_EDGE('',*,*,#4569,.T.);
#6391=ORIENTED_EDGE('',*,*,#4576,.F.);
#6392=ORIENTED_EDGE('',*,*,#4578,.T.);
#6393=ORIENTED_EDGE('',*,*,#4579,.T.);
#6394=ORIENTED_EDGE('',*,*,#4484,.T.);
#6395=ORIENTED_EDGE('',*,*,#4580,.T.);
#6396=ORIENTED_EDGE('',*,*,#4581,.T.);
#6397=ORIENTED_EDGE('',*,*,#4582,.T.);
#6398=ORIENTED_EDGE('',*,*,#4583,.T.);
#6399=ORIENTED_EDGE('',*,*,#4580,.F.);
#6400=ORIENTED_EDGE('',*,*,#4488,.T.);
#6401=ORIENTED_EDGE('',*,*,#4555,.F.);
#6402=ORIENTED_EDGE('',*,*,#4584,.T.);
#6403=ORIENTED_EDGE('',*,*,#4582,.F.);
#6404=ORIENTED_EDGE('',*,*,#4490,.T.);
#6405=ORIENTED_EDGE('',*,*,#4585,.T.);
#6406=ORIENTED_EDGE('',*,*,#4586,.T.);
#6407=ORIENTED_EDGE('',*,*,#4579,.F.);
#6408=ORIENTED_EDGE('',*,*,#4587,.T.);
#6409=ORIENTED_EDGE('',*,*,#4553,.F.);
#6410=ORIENTED_EDGE('',*,*,#4557,.F.);
#6411=ORIENTED_EDGE('',*,*,#4588,.F.);
#6412=ORIENTED_EDGE('',*,*,#4589,.F.);
#6413=ORIENTED_EDGE('',*,*,#4590,.F.);
#6414=ORIENTED_EDGE('',*,*,#4591,.F.);
#6415=ORIENTED_EDGE('',*,*,#4592,.F.);
#6416=ORIENTED_EDGE('',*,*,#4593,.T.);
#6417=ORIENTED_EDGE('',*,*,#4587,.F.);
#6418=ORIENTED_EDGE('',*,*,#4581,.F.);
#6419=ORIENTED_EDGE('',*,*,#4583,.F.);
#6420=ORIENTED_EDGE('',*,*,#4584,.F.);
#6421=ORIENTED_EDGE('',*,*,#4594,.T.);
#6422=ORIENTED_EDGE('',*,*,#4595,.T.);
#6423=ORIENTED_EDGE('',*,*,#4596,.T.);
#6424=ORIENTED_EDGE('',*,*,#4588,.T.);
#6425=ORIENTED_EDGE('',*,*,#4556,.F.);
#6426=ORIENTED_EDGE('',*,*,#4520,.T.);
#6427=ORIENTED_EDGE('',*,*,#4597,.T.);
#6428=ORIENTED_EDGE('',*,*,#4589,.T.);
#6429=ORIENTED_EDGE('',*,*,#4596,.F.);
#6430=ORIENTED_EDGE('',*,*,#4524,.T.);
#6431=ORIENTED_EDGE('',*,*,#4598,.T.);
#6432=ORIENTED_EDGE('',*,*,#4590,.T.);
#6433=ORIENTED_EDGE('',*,*,#4597,.F.);
#6434=ORIENTED_EDGE('',*,*,#4599,.T.);
#6435=ORIENTED_EDGE('',*,*,#4578,.F.);
#6436=ORIENTED_EDGE('',*,*,#4485,.F.);
#6437=ORIENTED_EDGE('',*,*,#4586,.F.);
#6438=ORIENTED_EDGE('',*,*,#4600,.F.);
#6439=ORIENTED_EDGE('',*,*,#4565,.F.);
#6440=ORIENTED_EDGE('',*,*,#4601,.T.);
#6441=ORIENTED_EDGE('',*,*,#4599,.F.);
#6442=ORIENTED_EDGE('',*,*,#4523,.T.);
#6443=ORIENTED_EDGE('',*,*,#4600,.T.);
#6444=ORIENTED_EDGE('',*,*,#4602,.F.);
#6445=ORIENTED_EDGE('',*,*,#4603,.F.);
#6446=ORIENTED_EDGE('',*,*,#4604,.T.);
#6447=ORIENTED_EDGE('',*,*,#4601,.F.);
#6448=ORIENTED_EDGE('',*,*,#4605,.F.);
#6449=ORIENTED_EDGE('',*,*,#4606,.F.);
#6450=ORIENTED_EDGE('',*,*,#4607,.T.);
#6451=ORIENTED_EDGE('',*,*,#4573,.F.);
#6452=ORIENTED_EDGE('',*,*,#4608,.T.);
#6453=ORIENTED_EDGE('',*,*,#4609,.F.);
#6454=ORIENTED_EDGE('',*,*,#4610,.T.);
#6455=ORIENTED_EDGE('',*,*,#4574,.F.);
#6456=ORIENTED_EDGE('',*,*,#4610,.F.);
#6457=ORIENTED_EDGE('',*,*,#4611,.F.);
#6458=ORIENTED_EDGE('',*,*,#4608,.F.);
#6459=ORIENTED_EDGE('',*,*,#4609,.T.);
#6460=ORIENTED_EDGE('',*,*,#4611,.T.);
#6461=ORIENTED_EDGE('',*,*,#4594,.F.);
#6462=ORIENTED_EDGE('',*,*,#4612,.F.);
#6463=ORIENTED_EDGE('',*,*,#4613,.F.);
#6464=ORIENTED_EDGE('',*,*,#4614,.F.);
#6465=ORIENTED_EDGE('',*,*,#4615,.T.);
#6466=ORIENTED_EDGE('',*,*,#4613,.T.);
#6467=ORIENTED_EDGE('',*,*,#4595,.F.);
#6468=ORIENTED_EDGE('',*,*,#4614,.T.);
#6469=ORIENTED_EDGE('',*,*,#4615,.F.);
#6470=ORIENTED_EDGE('',*,*,#4612,.T.);
#6471=ORIENTED_EDGE('',*,*,#4585,.F.);
#6472=ORIENTED_EDGE('',*,*,#4593,.F.);
#6473=ORIENTED_EDGE('',*,*,#4616,.F.);
#6474=ORIENTED_EDGE('',*,*,#4602,.T.);
#6475=ORIENTED_EDGE('',*,*,#4598,.F.);
#6476=ORIENTED_EDGE('',*,*,#4607,.F.);
#6477=ORIENTED_EDGE('',*,*,#4617,.F.);
#6478=ORIENTED_EDGE('',*,*,#4591,.T.);
#6479=ORIENTED_EDGE('',*,*,#4564,.F.);
#6480=ORIENTED_EDGE('',*,*,#4572,.F.);
#6481=ORIENTED_EDGE('',*,*,#4618,.F.);
#6482=ORIENTED_EDGE('',*,*,#4605,.T.);
#6483=ORIENTED_EDGE('',*,*,#4577,.F.);
#6484=ORIENTED_EDGE('',*,*,#4604,.F.);
#6485=ORIENTED_EDGE('',*,*,#4619,.F.);
#6486=ORIENTED_EDGE('',*,*,#4570,.T.);
#6487=ORIENTED_EDGE('',*,*,#4446,.F.);
#6488=ORIENTED_EDGE('',*,*,#4620,.F.);
#6489=ORIENTED_EDGE('',*,*,#4621,.T.);
#6490=ORIENTED_EDGE('',*,*,#4455,.T.);
#6491=ORIENTED_EDGE('',*,*,#4438,.F.);
#6492=ORIENTED_EDGE('',*,*,#4622,.F.);
#6493=ORIENTED_EDGE('',*,*,#4623,.T.);
#6494=ORIENTED_EDGE('',*,*,#4620,.T.);
#6495=ORIENTED_EDGE('',*,*,#4441,.F.);
#6496=ORIENTED_EDGE('',*,*,#4624,.F.);
#6497=ORIENTED_EDGE('',*,*,#4625,.T.);
#6498=ORIENTED_EDGE('',*,*,#4622,.T.);
#6499=ORIENTED_EDGE('',*,*,#4433,.F.);
#6500=ORIENTED_EDGE('',*,*,#4450,.F.);
#6501=ORIENTED_EDGE('',*,*,#4626,.T.);
#6502=ORIENTED_EDGE('',*,*,#4624,.T.);
#6503=ORIENTED_EDGE('',*,*,#4626,.F.);
#6504=ORIENTED_EDGE('',*,*,#4449,.F.);
#6505=ORIENTED_EDGE('',*,*,#4452,.F.);
#6506=ORIENTED_EDGE('',*,*,#4454,.F.);
#6507=ORIENTED_EDGE('',*,*,#4456,.F.);
#6508=ORIENTED_EDGE('',*,*,#4621,.F.);
#6509=ORIENTED_EDGE('',*,*,#4623,.F.);
#6510=ORIENTED_EDGE('',*,*,#4625,.F.);
#6511=ORIENTED_EDGE('',*,*,#4603,.T.);
#6512=ORIENTED_EDGE('',*,*,#4616,.T.);
#6513=ORIENTED_EDGE('',*,*,#4592,.T.);
#6514=ORIENTED_EDGE('',*,*,#4617,.T.);
#6515=ORIENTED_EDGE('',*,*,#4606,.T.);
#6516=ORIENTED_EDGE('',*,*,#4618,.T.);
#6517=ORIENTED_EDGE('',*,*,#4571,.T.);
#6518=ORIENTED_EDGE('',*,*,#4619,.T.);
#6519=ORIENTED_EDGE('',*,*,#4627,.T.);
#6520=ORIENTED_EDGE('',*,*,#4628,.T.);
#6521=ORIENTED_EDGE('',*,*,#4629,.T.);
#6522=ORIENTED_EDGE('',*,*,#4628,.F.);
#6523=ORIENTED_EDGE('',*,*,#4630,.F.);
#6524=ORIENTED_EDGE('',*,*,#4631,.T.);
#6525=ORIENTED_EDGE('',*,*,#4629,.F.);
#6526=ORIENTED_EDGE('',*,*,#4631,.F.);
#6527=ORIENTED_EDGE('',*,*,#4632,.T.);
#6528=ORIENTED_EDGE('',*,*,#4627,.F.);
#6529=ORIENTED_EDGE('',*,*,#4633,.T.);
#6530=ORIENTED_EDGE('',*,*,#4634,.T.);
#6531=ORIENTED_EDGE('',*,*,#4630,.T.);
#6532=ORIENTED_EDGE('',*,*,#4634,.F.);
#6533=ORIENTED_EDGE('',*,*,#4635,.T.);
#6534=ORIENTED_EDGE('',*,*,#4633,.F.);
#6535=ORIENTED_EDGE('',*,*,#4635,.F.);
#6536=ORIENTED_EDGE('',*,*,#4636,.T.);
#6537=ORIENTED_EDGE('',*,*,#4632,.F.);
#6538=ORIENTED_EDGE('',*,*,#4636,.F.);
#6539=ORIENTED_EDGE('',*,*,#4637,.F.);
#6540=ORIENTED_EDGE('',*,*,#4638,.F.);
#6541=ORIENTED_EDGE('',*,*,#4639,.T.);
#6542=ORIENTED_EDGE('',*,*,#4640,.F.);
#6543=ORIENTED_EDGE('',*,*,#4641,.T.);
#6544=ORIENTED_EDGE('',*,*,#4642,.F.);
#6545=ORIENTED_EDGE('',*,*,#4643,.F.);
#6546=ORIENTED_EDGE('',*,*,#4644,.F.);
#6547=ORIENTED_EDGE('',*,*,#4645,.T.);
#6548=ORIENTED_EDGE('',*,*,#4646,.T.);
#6549=ORIENTED_EDGE('',*,*,#4638,.T.);
#6550=ORIENTED_EDGE('',*,*,#4647,.T.);
#6551=ORIENTED_EDGE('',*,*,#4648,.T.);
#6552=ORIENTED_EDGE('',*,*,#4649,.T.);
#6553=ORIENTED_EDGE('',*,*,#4645,.F.);
#6554=ORIENTED_EDGE('',*,*,#4650,.T.);
#6555=ORIENTED_EDGE('',*,*,#4651,.T.);
#6556=ORIENTED_EDGE('',*,*,#4652,.T.);
#6557=ORIENTED_EDGE('',*,*,#4648,.F.);
#6558=ORIENTED_EDGE('',*,*,#4653,.T.);
#6559=ORIENTED_EDGE('',*,*,#4654,.T.);
#6560=ORIENTED_EDGE('',*,*,#4655,.T.);
#6561=ORIENTED_EDGE('',*,*,#4651,.F.);
#6562=ORIENTED_EDGE('',*,*,#4656,.T.);
#6563=ORIENTED_EDGE('',*,*,#4642,.T.);
#6564=ORIENTED_EDGE('',*,*,#4657,.T.);
#6565=ORIENTED_EDGE('',*,*,#4654,.F.);
#6566=ORIENTED_EDGE('',*,*,#4658,.T.);
#6567=ORIENTED_EDGE('',*,*,#4643,.T.);
#6568=ORIENTED_EDGE('',*,*,#4659,.T.);
#6569=ORIENTED_EDGE('',*,*,#4637,.T.);
#6570=ORIENTED_EDGE('',*,*,#4660,.T.);
#6571=ORIENTED_EDGE('',*,*,#4640,.T.);
#6572=ORIENTED_EDGE('',*,*,#4661,.T.);
#6573=ORIENTED_EDGE('',*,*,#4662,.T.);
#6574=ORIENTED_EDGE('',*,*,#4644,.T.);
#6575=ORIENTED_EDGE('',*,*,#4663,.T.);
#6576=ORIENTED_EDGE('',*,*,#4652,.F.);
#6577=ORIENTED_EDGE('',*,*,#4664,.F.);
#6578=ORIENTED_EDGE('',*,*,#4665,.F.);
#6579=ORIENTED_EDGE('',*,*,#4666,.F.);
#6580=ORIENTED_EDGE('',*,*,#4655,.F.);
#6581=ORIENTED_EDGE('',*,*,#4667,.T.);
#6582=ORIENTED_EDGE('',*,*,#4668,.F.);
#6583=ORIENTED_EDGE('',*,*,#4664,.T.);
#6584=ORIENTED_EDGE('',*,*,#4647,.F.);
#6585=ORIENTED_EDGE('',*,*,#4659,.F.);
#6586=ORIENTED_EDGE('',*,*,#4658,.F.);
#6587=ORIENTED_EDGE('',*,*,#4656,.F.);
#6588=ORIENTED_EDGE('',*,*,#4653,.F.);
#6589=ORIENTED_EDGE('',*,*,#4650,.F.);
#6590=ORIENTED_EDGE('',*,*,#4669,.T.);
#6591=ORIENTED_EDGE('',*,*,#4660,.F.);
#6592=ORIENTED_EDGE('',*,*,#4663,.F.);
#6593=ORIENTED_EDGE('',*,*,#4670,.T.);
#6594=ORIENTED_EDGE('',*,*,#4671,.F.);
#6595=ORIENTED_EDGE('',*,*,#4672,.F.);
#6596=ORIENTED_EDGE('',*,*,#4673,.F.);
#6597=ORIENTED_EDGE('',*,*,#4674,.F.);
#6598=ORIENTED_EDGE('',*,*,#4675,.F.);
#6599=ORIENTED_EDGE('',*,*,#4676,.T.);
#6600=ORIENTED_EDGE('',*,*,#4677,.F.);
#6601=ORIENTED_EDGE('',*,*,#4678,.T.);
#6602=ORIENTED_EDGE('',*,*,#4679,.T.);
#6603=ORIENTED_EDGE('',*,*,#4675,.T.);
#6604=ORIENTED_EDGE('',*,*,#4680,.T.);
#6605=ORIENTED_EDGE('',*,*,#4681,.T.);
#6606=ORIENTED_EDGE('',*,*,#4668,.T.);
#6607=ORIENTED_EDGE('',*,*,#4678,.F.);
#6608=ORIENTED_EDGE('',*,*,#4682,.T.);
#6609=ORIENTED_EDGE('',*,*,#4683,.T.);
#6610=ORIENTED_EDGE('',*,*,#4665,.T.);
#6611=ORIENTED_EDGE('',*,*,#4681,.F.);
#6612=ORIENTED_EDGE('',*,*,#4684,.T.);
#6613=ORIENTED_EDGE('',*,*,#4685,.T.);
#6614=ORIENTED_EDGE('',*,*,#4686,.T.);
#6615=ORIENTED_EDGE('',*,*,#4683,.F.);
#6616=ORIENTED_EDGE('',*,*,#4687,.T.);
#6617=ORIENTED_EDGE('',*,*,#4671,.T.);
#6618=ORIENTED_EDGE('',*,*,#4688,.T.);
#6619=ORIENTED_EDGE('',*,*,#4685,.F.);
#6620=ORIENTED_EDGE('',*,*,#4689,.T.);
#6621=ORIENTED_EDGE('',*,*,#4677,.T.);
#6622=ORIENTED_EDGE('',*,*,#4690,.T.);
#6623=ORIENTED_EDGE('',*,*,#4673,.T.);
#6624=ORIENTED_EDGE('',*,*,#4691,.T.);
#6625=ORIENTED_EDGE('',*,*,#4672,.T.);
#6626=ORIENTED_EDGE('',*,*,#4692,.T.);
#6627=ORIENTED_EDGE('',*,*,#4674,.T.);
#6628=ORIENTED_EDGE('',*,*,#4693,.T.);
#6629=ORIENTED_EDGE('',*,*,#4646,.F.);
#6630=ORIENTED_EDGE('',*,*,#4694,.F.);
#6631=ORIENTED_EDGE('',*,*,#4688,.F.);
#6632=ORIENTED_EDGE('',*,*,#4670,.F.);
#6633=ORIENTED_EDGE('',*,*,#4690,.F.);
#6634=ORIENTED_EDGE('',*,*,#4676,.F.);
#6635=ORIENTED_EDGE('',*,*,#4679,.F.);
#6636=ORIENTED_EDGE('',*,*,#4667,.F.);
#6637=ORIENTED_EDGE('',*,*,#4657,.F.);
#6638=ORIENTED_EDGE('',*,*,#4641,.F.);
#6639=ORIENTED_EDGE('',*,*,#4662,.F.);
#6640=ORIENTED_EDGE('',*,*,#4695,.T.);
#6641=ORIENTED_EDGE('',*,*,#4696,.F.);
#6642=ORIENTED_EDGE('',*,*,#4695,.F.);
#6643=ORIENTED_EDGE('',*,*,#4661,.F.);
#6644=ORIENTED_EDGE('',*,*,#4639,.F.);
#6645=ORIENTED_EDGE('',*,*,#4680,.F.);
#6646=ORIENTED_EDGE('',*,*,#4692,.F.);
#6647=ORIENTED_EDGE('',*,*,#4689,.F.);
#6648=ORIENTED_EDGE('',*,*,#4687,.F.);
#6649=ORIENTED_EDGE('',*,*,#4684,.F.);
#6650=ORIENTED_EDGE('',*,*,#4682,.F.);
#6651=ORIENTED_EDGE('',*,*,#4697,.T.);
#6652=ORIENTED_EDGE('',*,*,#4691,.F.);
#6653=ORIENTED_EDGE('',*,*,#4693,.F.);
#6654=ORIENTED_EDGE('',*,*,#4649,.F.);
#6655=ORIENTED_EDGE('',*,*,#4666,.T.);
#6656=ORIENTED_EDGE('',*,*,#4686,.F.);
#6657=ORIENTED_EDGE('',*,*,#4694,.T.);
#6658=ORIENTED_EDGE('',*,*,#4696,.T.);
#6659=ORIENTED_EDGE('',*,*,#4698,.T.);
#6660=ORIENTED_EDGE('',*,*,#4699,.T.);
#6661=ORIENTED_EDGE('',*,*,#4698,.F.);
#6662=ORIENTED_EDGE('',*,*,#4699,.F.);
#6663=ORIENTED_EDGE('',*,*,#4700,.F.);
#6664=ORIENTED_EDGE('',*,*,#4701,.T.);
#6665=ORIENTED_EDGE('',*,*,#4702,.T.);
#6666=ORIENTED_EDGE('',*,*,#4700,.T.);
#6667=ORIENTED_EDGE('',*,*,#4702,.F.);
#6668=ORIENTED_EDGE('',*,*,#4703,.F.);
#6669=ORIENTED_EDGE('',*,*,#4704,.T.);
#6670=ORIENTED_EDGE('',*,*,#4701,.F.);
#6671=ORIENTED_EDGE('',*,*,#4704,.F.);
#6672=ORIENTED_EDGE('',*,*,#4705,.F.);
#6673=ORIENTED_EDGE('',*,*,#4706,.T.);
#6674=ORIENTED_EDGE('',*,*,#4707,.T.);
#6675=ORIENTED_EDGE('',*,*,#4705,.T.);
#6676=ORIENTED_EDGE('',*,*,#4703,.T.);
#6677=ORIENTED_EDGE('',*,*,#4707,.F.);
#6678=ORIENTED_EDGE('',*,*,#4706,.F.);
#6679=ORIENTED_EDGE('',*,*,#4708,.F.);
#6680=ORIENTED_EDGE('',*,*,#4708,.T.);
#6681=ORIENTED_EDGE('',*,*,#4709,.T.);
#6682=ORIENTED_EDGE('',*,*,#4710,.T.);
#6683=ORIENTED_EDGE('',*,*,#4709,.F.);
#6684=ORIENTED_EDGE('',*,*,#4710,.F.);
#6685=ORIENTED_EDGE('',*,*,#4711,.T.);
#6686=ORIENTED_EDGE('',*,*,#4712,.F.);
#6687=ORIENTED_EDGE('',*,*,#4711,.F.);
#6688=ORIENTED_EDGE('',*,*,#4669,.F.);
#6689=ORIENTED_EDGE('',*,*,#4713,.T.);
#6690=ORIENTED_EDGE('',*,*,#4697,.F.);
#6691=ORIENTED_EDGE('',*,*,#4713,.F.);
#6692=ORIENTED_EDGE('',*,*,#4712,.T.);
#6693=ORIENTED_EDGE('',*,*,#4714,.F.);
#6694=ORIENTED_EDGE('',*,*,#4715,.T.);
#6695=ORIENTED_EDGE('',*,*,#4716,.T.);
#6696=ORIENTED_EDGE('',*,*,#4717,.T.);
#6697=ORIENTED_EDGE('',*,*,#4718,.F.);
#6698=ORIENTED_EDGE('',*,*,#4719,.T.);
#6699=ORIENTED_EDGE('',*,*,#4714,.T.);
#6700=ORIENTED_EDGE('',*,*,#4720,.T.);
#6701=ORIENTED_EDGE('',*,*,#4721,.F.);
#6702=ORIENTED_EDGE('',*,*,#4722,.T.);
#6703=ORIENTED_EDGE('',*,*,#4718,.T.);
#6704=ORIENTED_EDGE('',*,*,#4723,.T.);
#6705=ORIENTED_EDGE('',*,*,#4724,.F.);
#6706=ORIENTED_EDGE('',*,*,#4725,.T.);
#6707=ORIENTED_EDGE('',*,*,#4721,.T.);
#6708=ORIENTED_EDGE('',*,*,#4726,.T.);
#6709=ORIENTED_EDGE('',*,*,#4727,.F.);
#6710=ORIENTED_EDGE('',*,*,#4728,.T.);
#6711=ORIENTED_EDGE('',*,*,#4724,.T.);
#6712=ORIENTED_EDGE('',*,*,#4729,.T.);
#6713=ORIENTED_EDGE('',*,*,#4730,.F.);
#6714=ORIENTED_EDGE('',*,*,#4731,.T.);
#6715=ORIENTED_EDGE('',*,*,#4727,.T.);
#6716=ORIENTED_EDGE('',*,*,#4732,.T.);
#6717=ORIENTED_EDGE('',*,*,#4733,.F.);
#6718=ORIENTED_EDGE('',*,*,#4734,.T.);
#6719=ORIENTED_EDGE('',*,*,#4735,.F.);
#6720=ORIENTED_EDGE('',*,*,#4736,.F.);
#6721=ORIENTED_EDGE('',*,*,#4737,.F.);
#6722=ORIENTED_EDGE('',*,*,#4738,.T.);
#6723=ORIENTED_EDGE('',*,*,#4733,.T.);
#6724=ORIENTED_EDGE('',*,*,#4739,.F.);
#6725=ORIENTED_EDGE('',*,*,#4740,.F.);
#6726=ORIENTED_EDGE('',*,*,#4741,.T.);
#6727=ORIENTED_EDGE('',*,*,#4737,.T.);
#6728=ORIENTED_EDGE('',*,*,#4742,.F.);
#6729=ORIENTED_EDGE('',*,*,#4743,.F.);
#6730=ORIENTED_EDGE('',*,*,#4744,.T.);
#6731=ORIENTED_EDGE('',*,*,#4740,.T.);
#6732=ORIENTED_EDGE('',*,*,#4745,.F.);
#6733=ORIENTED_EDGE('',*,*,#4746,.F.);
#6734=ORIENTED_EDGE('',*,*,#4747,.T.);
#6735=ORIENTED_EDGE('',*,*,#4743,.T.);
#6736=ORIENTED_EDGE('',*,*,#4748,.F.);
#6737=ORIENTED_EDGE('',*,*,#4749,.F.);
#6738=ORIENTED_EDGE('',*,*,#4750,.F.);
#6739=ORIENTED_EDGE('',*,*,#4732,.F.);
#6740=ORIENTED_EDGE('',*,*,#4729,.F.);
#6741=ORIENTED_EDGE('',*,*,#4726,.F.);
#6742=ORIENTED_EDGE('',*,*,#4723,.F.);
#6743=ORIENTED_EDGE('',*,*,#4720,.F.);
#6744=ORIENTED_EDGE('',*,*,#4717,.F.);
#6745=ORIENTED_EDGE('',*,*,#4751,.F.);
#6746=ORIENTED_EDGE('',*,*,#4752,.T.);
#6747=ORIENTED_EDGE('',*,*,#4748,.T.);
#6748=ORIENTED_EDGE('',*,*,#4745,.T.);
#6749=ORIENTED_EDGE('',*,*,#4742,.T.);
#6750=ORIENTED_EDGE('',*,*,#4739,.T.);
#6751=ORIENTED_EDGE('',*,*,#4736,.T.);
#6752=ORIENTED_EDGE('',*,*,#4746,.T.);
#6753=ORIENTED_EDGE('',*,*,#4752,.F.);
#6754=ORIENTED_EDGE('',*,*,#4753,.F.);
#6755=ORIENTED_EDGE('',*,*,#4754,.T.);
#6756=ORIENTED_EDGE('',*,*,#4755,.F.);
#6757=ORIENTED_EDGE('',*,*,#4734,.F.);
#6758=ORIENTED_EDGE('',*,*,#4738,.F.);
#6759=ORIENTED_EDGE('',*,*,#4741,.F.);
#6760=ORIENTED_EDGE('',*,*,#4744,.F.);
#6761=ORIENTED_EDGE('',*,*,#4747,.F.);
#6762=ORIENTED_EDGE('',*,*,#4754,.F.);
#6763=ORIENTED_EDGE('',*,*,#4756,.F.);
#6764=ORIENTED_EDGE('',*,*,#4715,.F.);
#6765=ORIENTED_EDGE('',*,*,#4719,.F.);
#6766=ORIENTED_EDGE('',*,*,#4722,.F.);
#6767=ORIENTED_EDGE('',*,*,#4725,.F.);
#6768=ORIENTED_EDGE('',*,*,#4728,.F.);
#6769=ORIENTED_EDGE('',*,*,#4731,.F.);
#6770=ORIENTED_EDGE('',*,*,#4757,.F.);
#6771=ORIENTED_EDGE('',*,*,#4758,.F.);
#6772=ORIENTED_EDGE('',*,*,#4759,.T.);
#6773=ORIENTED_EDGE('',*,*,#4749,.T.);
#6774=ORIENTED_EDGE('',*,*,#4735,.T.);
#6775=ORIENTED_EDGE('',*,*,#4755,.T.);
#6776=ORIENTED_EDGE('',*,*,#4760,.F.);
#6777=ORIENTED_EDGE('',*,*,#4761,.T.);
#6778=ORIENTED_EDGE('',*,*,#4758,.T.);
#6779=ORIENTED_EDGE('',*,*,#4761,.F.);
#6780=ORIENTED_EDGE('',*,*,#4760,.T.);
#6781=ORIENTED_EDGE('',*,*,#4762,.T.);
#6782=ORIENTED_EDGE('',*,*,#4751,.T.);
#6783=ORIENTED_EDGE('',*,*,#4716,.F.);
#6784=ORIENTED_EDGE('',*,*,#4756,.T.);
#6785=ORIENTED_EDGE('',*,*,#4753,.T.);
#6786=ORIENTED_EDGE('',*,*,#4763,.F.);
#6787=ORIENTED_EDGE('',*,*,#4762,.F.);
#6788=ORIENTED_EDGE('',*,*,#4764,.T.);
#6789=ORIENTED_EDGE('',*,*,#4763,.T.);
#6790=ORIENTED_EDGE('',*,*,#4764,.F.);
#6791=ORIENTED_EDGE('',*,*,#4730,.T.);
#6792=ORIENTED_EDGE('',*,*,#4750,.T.);
#6793=ORIENTED_EDGE('',*,*,#4759,.F.);
#6794=ORIENTED_EDGE('',*,*,#4757,.T.);
#6795=ORIENTED_EDGE('',*,*,#4765,.T.);
#6796=ORIENTED_EDGE('',*,*,#4766,.T.);
#6797=ORIENTED_EDGE('',*,*,#4767,.T.);
#6798=ORIENTED_EDGE('',*,*,#4768,.T.);
#6799=ORIENTED_EDGE('',*,*,#4769,.T.);
#6800=ORIENTED_EDGE('',*,*,#4770,.T.);
#6801=ORIENTED_EDGE('',*,*,#4771,.T.);
#6802=ORIENTED_EDGE('',*,*,#4772,.T.);
#6803=ORIENTED_EDGE('',*,*,#4773,.T.);
#6804=ORIENTED_EDGE('',*,*,#4774,.T.);
#6805=ORIENTED_EDGE('',*,*,#4775,.T.);
#6806=ORIENTED_EDGE('',*,*,#4776,.T.);
#6807=ORIENTED_EDGE('',*,*,#4765,.F.);
#6808=ORIENTED_EDGE('',*,*,#4777,.T.);
#6809=ORIENTED_EDGE('',*,*,#4775,.F.);
#6810=ORIENTED_EDGE('',*,*,#4778,.T.);
#6811=ORIENTED_EDGE('',*,*,#4772,.F.);
#6812=ORIENTED_EDGE('',*,*,#4779,.T.);
#6813=ORIENTED_EDGE('',*,*,#4774,.F.);
#6814=ORIENTED_EDGE('',*,*,#4780,.T.);
#6815=ORIENTED_EDGE('',*,*,#4769,.F.);
#6816=ORIENTED_EDGE('',*,*,#4781,.T.);
#6817=ORIENTED_EDGE('',*,*,#4771,.F.);
#6818=ORIENTED_EDGE('',*,*,#4782,.T.);
#6819=ORIENTED_EDGE('',*,*,#4766,.F.);
#6820=ORIENTED_EDGE('',*,*,#4783,.T.);
#6821=ORIENTED_EDGE('',*,*,#4768,.F.);
#6822=ORIENTED_EDGE('',*,*,#4784,.T.);
#6823=ORIENTED_EDGE('',*,*,#4782,.F.);
#6824=ORIENTED_EDGE('',*,*,#4785,.F.);
#6825=ORIENTED_EDGE('',*,*,#4786,.T.);
#6826=ORIENTED_EDGE('',*,*,#4787,.T.);
#6827=ORIENTED_EDGE('',*,*,#4773,.F.);
#6828=ORIENTED_EDGE('',*,*,#4788,.F.);
#6829=ORIENTED_EDGE('',*,*,#4789,.T.);
#6830=ORIENTED_EDGE('',*,*,#4785,.T.);
#6831=ORIENTED_EDGE('',*,*,#4780,.F.);
#6832=ORIENTED_EDGE('',*,*,#4790,.F.);
#6833=ORIENTED_EDGE('',*,*,#4791,.T.);
#6834=ORIENTED_EDGE('',*,*,#4788,.T.);
#6835=ORIENTED_EDGE('',*,*,#4776,.F.);
#6836=ORIENTED_EDGE('',*,*,#4792,.F.);
#6837=ORIENTED_EDGE('',*,*,#4793,.T.);
#6838=ORIENTED_EDGE('',*,*,#4790,.T.);
#6839=ORIENTED_EDGE('',*,*,#4778,.F.);
#6840=ORIENTED_EDGE('',*,*,#4779,.F.);
#6841=ORIENTED_EDGE('',*,*,#4781,.F.);
#6842=ORIENTED_EDGE('',*,*,#4783,.F.);
#6843=ORIENTED_EDGE('',*,*,#4794,.T.);
#6844=ORIENTED_EDGE('',*,*,#4795,.T.);
#6845=ORIENTED_EDGE('',*,*,#4796,.T.);
#6846=ORIENTED_EDGE('',*,*,#4797,.T.);
#6847=ORIENTED_EDGE('',*,*,#4798,.T.);
#6848=ORIENTED_EDGE('',*,*,#4799,.T.);
#6849=ORIENTED_EDGE('',*,*,#4800,.F.);
#6850=ORIENTED_EDGE('',*,*,#4801,.F.);
#6851=ORIENTED_EDGE('',*,*,#4802,.T.);
#6852=ORIENTED_EDGE('',*,*,#4803,.T.);
#6853=ORIENTED_EDGE('',*,*,#4804,.F.);
#6854=ORIENTED_EDGE('',*,*,#4799,.F.);
#6855=ORIENTED_EDGE('',*,*,#4805,.T.);
#6856=ORIENTED_EDGE('',*,*,#4806,.T.);
#6857=ORIENTED_EDGE('',*,*,#4807,.F.);
#6858=ORIENTED_EDGE('',*,*,#4803,.F.);
#6859=ORIENTED_EDGE('',*,*,#4808,.T.);
#6860=ORIENTED_EDGE('',*,*,#4809,.T.);
#6861=ORIENTED_EDGE('',*,*,#4810,.F.);
#6862=ORIENTED_EDGE('',*,*,#4806,.F.);
#6863=ORIENTED_EDGE('',*,*,#4811,.T.);
#6864=ORIENTED_EDGE('',*,*,#4801,.T.);
#6865=ORIENTED_EDGE('',*,*,#4812,.F.);
#6866=ORIENTED_EDGE('',*,*,#4813,.F.);
#6867=ORIENTED_EDGE('',*,*,#4814,.T.);
#6868=ORIENTED_EDGE('',*,*,#4813,.T.);
#6869=ORIENTED_EDGE('',*,*,#4815,.F.);
#6870=ORIENTED_EDGE('',*,*,#4816,.F.);
#6871=ORIENTED_EDGE('',*,*,#4817,.T.);
#6872=ORIENTED_EDGE('',*,*,#4816,.T.);
#6873=ORIENTED_EDGE('',*,*,#4818,.F.);
#6874=ORIENTED_EDGE('',*,*,#4819,.F.);
#6875=ORIENTED_EDGE('',*,*,#4820,.T.);
#6876=ORIENTED_EDGE('',*,*,#4819,.T.);
#6877=ORIENTED_EDGE('',*,*,#4821,.F.);
#6878=ORIENTED_EDGE('',*,*,#4809,.F.);
#6879=ORIENTED_EDGE('',*,*,#4810,.T.);
#6880=ORIENTED_EDGE('',*,*,#4821,.T.);
#6881=ORIENTED_EDGE('',*,*,#4818,.T.);
#6882=ORIENTED_EDGE('',*,*,#4815,.T.);
#6883=ORIENTED_EDGE('',*,*,#4812,.T.);
#6884=ORIENTED_EDGE('',*,*,#4800,.T.);
#6885=ORIENTED_EDGE('',*,*,#4804,.T.);
#6886=ORIENTED_EDGE('',*,*,#4807,.T.);
#6887=ORIENTED_EDGE('',*,*,#4822,.T.);
#6888=ORIENTED_EDGE('',*,*,#4823,.T.);
#6889=ORIENTED_EDGE('',*,*,#4824,.T.);
#6890=ORIENTED_EDGE('',*,*,#4825,.T.);
#6891=ORIENTED_EDGE('',*,*,#4808,.F.);
#6892=ORIENTED_EDGE('',*,*,#4805,.F.);
#6893=ORIENTED_EDGE('',*,*,#4802,.F.);
#6894=ORIENTED_EDGE('',*,*,#4798,.F.);
#6895=ORIENTED_EDGE('',*,*,#4811,.F.);
#6896=ORIENTED_EDGE('',*,*,#4814,.F.);
#6897=ORIENTED_EDGE('',*,*,#4817,.F.);
#6898=ORIENTED_EDGE('',*,*,#4820,.F.);
#6899=ORIENTED_EDGE('',*,*,#4826,.F.);
#6900=ORIENTED_EDGE('',*,*,#4827,.F.);
#6901=ORIENTED_EDGE('',*,*,#4786,.F.);
#6902=ORIENTED_EDGE('',*,*,#4789,.F.);
#6903=ORIENTED_EDGE('',*,*,#4791,.F.);
#6904=ORIENTED_EDGE('',*,*,#4793,.F.);
#6905=ORIENTED_EDGE('',*,*,#4828,.F.);
#6906=ORIENTED_EDGE('',*,*,#4829,.F.);
#6907=ORIENTED_EDGE('',*,*,#4830,.F.);
#6908=ORIENTED_EDGE('',*,*,#4797,.F.);
#6909=ORIENTED_EDGE('',*,*,#4831,.F.);
#6910=ORIENTED_EDGE('',*,*,#4823,.F.);
#6911=ORIENTED_EDGE('',*,*,#4831,.T.);
#6912=ORIENTED_EDGE('',*,*,#4796,.F.);
#6913=ORIENTED_EDGE('',*,*,#4832,.F.);
#6914=ORIENTED_EDGE('',*,*,#4824,.F.);
#6915=ORIENTED_EDGE('',*,*,#4832,.T.);
#6916=ORIENTED_EDGE('',*,*,#4795,.F.);
#6917=ORIENTED_EDGE('',*,*,#4833,.F.);
#6918=ORIENTED_EDGE('',*,*,#4825,.F.);
#6919=ORIENTED_EDGE('',*,*,#4833,.T.);
#6920=ORIENTED_EDGE('',*,*,#4794,.F.);
#6921=ORIENTED_EDGE('',*,*,#4830,.T.);
#6922=ORIENTED_EDGE('',*,*,#4822,.F.);
#6923=ORIENTED_EDGE('',*,*,#4784,.F.);
#6924=ORIENTED_EDGE('',*,*,#4834,.F.);
#6925=ORIENTED_EDGE('',*,*,#4826,.T.);
#6926=ORIENTED_EDGE('',*,*,#4835,.T.);
#6927=ORIENTED_EDGE('',*,*,#4770,.F.);
#6928=ORIENTED_EDGE('',*,*,#4787,.F.);
#6929=ORIENTED_EDGE('',*,*,#4827,.T.);
#6930=ORIENTED_EDGE('',*,*,#4834,.T.);
#6931=ORIENTED_EDGE('',*,*,#4777,.F.);
#6932=ORIENTED_EDGE('',*,*,#4836,.F.);
#6933=ORIENTED_EDGE('',*,*,#4828,.T.);
#6934=ORIENTED_EDGE('',*,*,#4792,.T.);
#6935=ORIENTED_EDGE('',*,*,#4767,.F.);
#6936=ORIENTED_EDGE('',*,*,#4835,.F.);
#6937=ORIENTED_EDGE('',*,*,#4829,.T.);
#6938=ORIENTED_EDGE('',*,*,#4836,.T.);
#6939=ORIENTED_EDGE('',*,*,#4837,.F.);
#6940=ORIENTED_EDGE('',*,*,#4838,.F.);
#6941=ORIENTED_EDGE('',*,*,#4839,.T.);
#6942=ORIENTED_EDGE('',*,*,#4840,.T.);
#6943=ORIENTED_EDGE('',*,*,#4841,.F.);
#6944=ORIENTED_EDGE('',*,*,#4842,.F.);
#6945=ORIENTED_EDGE('',*,*,#4843,.F.);
#6946=ORIENTED_EDGE('',*,*,#4842,.T.);
#6947=ORIENTED_EDGE('',*,*,#4844,.F.);
#6948=ORIENTED_EDGE('',*,*,#4845,.F.);
#6949=ORIENTED_EDGE('',*,*,#4844,.T.);
#6950=ORIENTED_EDGE('',*,*,#4841,.T.);
#6951=ORIENTED_EDGE('',*,*,#4846,.T.);
#6952=ORIENTED_EDGE('',*,*,#4847,.F.);
#6953=ORIENTED_EDGE('',*,*,#4848,.F.);
#6954=ORIENTED_EDGE('',*,*,#4849,.F.);
#6955=ORIENTED_EDGE('',*,*,#4848,.T.);
#6956=ORIENTED_EDGE('',*,*,#4850,.T.);
#6957=ORIENTED_EDGE('',*,*,#4851,.F.);
#6958=ORIENTED_EDGE('',*,*,#4850,.F.);
#6959=ORIENTED_EDGE('',*,*,#4847,.T.);
#6960=ORIENTED_EDGE('',*,*,#4852,.T.);
#6961=ORIENTED_EDGE('',*,*,#4853,.F.);
#6962=ORIENTED_EDGE('',*,*,#4854,.F.);
#6963=ORIENTED_EDGE('',*,*,#4855,.F.);
#6964=ORIENTED_EDGE('',*,*,#4854,.T.);
#6965=ORIENTED_EDGE('',*,*,#4856,.F.);
#6966=ORIENTED_EDGE('',*,*,#4857,.F.);
#6967=ORIENTED_EDGE('',*,*,#4856,.T.);
#6968=ORIENTED_EDGE('',*,*,#4853,.T.);
#6969=ORIENTED_EDGE('',*,*,#4858,.T.);
#6970=ORIENTED_EDGE('',*,*,#4859,.F.);
#6971=ORIENTED_EDGE('',*,*,#4860,.F.);
#6972=ORIENTED_EDGE('',*,*,#4861,.F.);
#6973=ORIENTED_EDGE('',*,*,#4860,.T.);
#6974=ORIENTED_EDGE('',*,*,#4862,.T.);
#6975=ORIENTED_EDGE('',*,*,#4863,.F.);
#6976=ORIENTED_EDGE('',*,*,#4864,.F.);
#6977=ORIENTED_EDGE('',*,*,#4865,.T.);
#6978=ORIENTED_EDGE('',*,*,#4866,.T.);
#6979=ORIENTED_EDGE('',*,*,#4867,.F.);
#6980=ORIENTED_EDGE('',*,*,#4868,.F.);
#6981=ORIENTED_EDGE('',*,*,#4869,.F.);
#6982=ORIENTED_EDGE('',*,*,#4868,.T.);
#6983=ORIENTED_EDGE('',*,*,#4870,.F.);
#6984=ORIENTED_EDGE('',*,*,#4871,.F.);
#6985=ORIENTED_EDGE('',*,*,#4862,.F.);
#6986=ORIENTED_EDGE('',*,*,#4859,.T.);
#6987=ORIENTED_EDGE('',*,*,#4872,.T.);
#6988=ORIENTED_EDGE('',*,*,#4873,.F.);
#6989=ORIENTED_EDGE('',*,*,#4874,.F.);
#6990=ORIENTED_EDGE('',*,*,#4875,.F.);
#6991=ORIENTED_EDGE('',*,*,#4874,.T.);
#6992=ORIENTED_EDGE('',*,*,#4876,.F.);
#6993=ORIENTED_EDGE('',*,*,#4877,.F.);
#6994=ORIENTED_EDGE('',*,*,#4878,.T.);
#6995=ORIENTED_EDGE('',*,*,#4838,.T.);
#6996=ORIENTED_EDGE('',*,*,#4879,.F.);
#6997=ORIENTED_EDGE('',*,*,#4870,.T.);
#6998=ORIENTED_EDGE('',*,*,#4867,.T.);
#6999=ORIENTED_EDGE('',*,*,#4880,.T.);
#7000=ORIENTED_EDGE('',*,*,#4839,.F.);
#7001=ORIENTED_EDGE('',*,*,#4878,.F.);
#7002=ORIENTED_EDGE('',*,*,#4881,.F.);
#7003=ORIENTED_EDGE('',*,*,#4882,.F.);
#7004=ORIENTED_EDGE('',*,*,#4883,.T.);
#7005=ORIENTED_EDGE('',*,*,#4864,.T.);
#7006=ORIENTED_EDGE('',*,*,#4884,.F.);
#7007=ORIENTED_EDGE('',*,*,#4876,.T.);
#7008=ORIENTED_EDGE('',*,*,#4873,.T.);
#7009=ORIENTED_EDGE('',*,*,#4885,.T.);
#7010=ORIENTED_EDGE('',*,*,#4865,.F.);
#7011=ORIENTED_EDGE('',*,*,#4883,.F.);
#7012=ORIENTED_EDGE('',*,*,#4846,.F.);
#7013=ORIENTED_EDGE('',*,*,#4840,.F.);
#7014=ORIENTED_EDGE('',*,*,#4880,.F.);
#7015=ORIENTED_EDGE('',*,*,#4866,.F.);
#7016=ORIENTED_EDGE('',*,*,#4885,.F.);
#7017=ORIENTED_EDGE('',*,*,#4872,.F.);
#7018=ORIENTED_EDGE('',*,*,#4858,.F.);
#7019=ORIENTED_EDGE('',*,*,#4852,.F.);
#7020=ORIENTED_EDGE('',*,*,#4886,.T.);
#7021=ORIENTED_EDGE('',*,*,#4887,.T.);
#7022=ORIENTED_EDGE('',*,*,#4888,.T.);
#7023=ORIENTED_EDGE('',*,*,#4887,.F.);
#7024=ORIENTED_EDGE('',*,*,#4889,.T.);
#7025=ORIENTED_EDGE('',*,*,#4886,.F.);
#7026=ORIENTED_EDGE('',*,*,#4890,.F.);
#7027=ORIENTED_EDGE('',*,*,#4891,.T.);
#7028=ORIENTED_EDGE('',*,*,#4888,.F.);
#7029=ORIENTED_EDGE('',*,*,#4891,.F.);
#7030=ORIENTED_EDGE('',*,*,#4892,.F.);
#7031=ORIENTED_EDGE('',*,*,#4893,.T.);
#7032=ORIENTED_EDGE('',*,*,#4890,.T.);
#7033=ORIENTED_EDGE('',*,*,#4893,.F.);
#7034=ORIENTED_EDGE('',*,*,#4894,.F.);
#7035=ORIENTED_EDGE('',*,*,#4895,.T.);
#7036=ORIENTED_EDGE('',*,*,#4892,.T.);
#7037=ORIENTED_EDGE('',*,*,#4895,.F.);
#7038=ORIENTED_EDGE('',*,*,#4894,.T.);
#7039=ORIENTED_EDGE('',*,*,#4871,.T.);
#7040=ORIENTED_EDGE('',*,*,#4875,.T.);
#7041=ORIENTED_EDGE('',*,*,#4884,.T.);
#7042=ORIENTED_EDGE('',*,*,#4882,.T.);
#7043=ORIENTED_EDGE('',*,*,#4863,.T.);
#7044=ORIENTED_EDGE('',*,*,#4869,.T.);
#7045=ORIENTED_EDGE('',*,*,#4879,.T.);
#7046=ORIENTED_EDGE('',*,*,#4896,.T.);
#7047=ORIENTED_EDGE('',*,*,#4897,.F.);
#7048=ORIENTED_EDGE('',*,*,#4898,.F.);
#7049=ORIENTED_EDGE('',*,*,#4896,.F.);
#7050=ORIENTED_EDGE('',*,*,#4881,.T.);
#7051=ORIENTED_EDGE('',*,*,#4877,.T.);
#7052=ORIENTED_EDGE('',*,*,#4837,.T.);
#7053=ORIENTED_EDGE('',*,*,#4843,.T.);
#7054=ORIENTED_EDGE('',*,*,#4845,.T.);
#7055=ORIENTED_EDGE('',*,*,#4849,.T.);
#7056=ORIENTED_EDGE('',*,*,#4851,.T.);
#7057=ORIENTED_EDGE('',*,*,#4855,.T.);
#7058=ORIENTED_EDGE('',*,*,#4857,.T.);
#7059=ORIENTED_EDGE('',*,*,#4861,.T.);
#7060=ORIENTED_EDGE('',*,*,#4889,.F.);
#7061=ORIENTED_EDGE('',*,*,#4899,.T.);
#7062=ORIENTED_EDGE('',*,*,#4897,.T.);
#7063=ORIENTED_EDGE('',*,*,#4898,.T.);
#7064=ORIENTED_EDGE('',*,*,#4899,.F.);
#7065=ORIENTED_EDGE('',*,*,#4900,.F.);
#7066=ORIENTED_EDGE('',*,*,#4901,.F.);
#7067=ORIENTED_EDGE('',*,*,#4902,.T.);
#7068=ORIENTED_EDGE('',*,*,#4903,.T.);
#7069=ORIENTED_EDGE('',*,*,#4904,.F.);
#7070=ORIENTED_EDGE('',*,*,#4905,.F.);
#7071=ORIENTED_EDGE('',*,*,#4906,.F.);
#7072=ORIENTED_EDGE('',*,*,#4905,.T.);
#7073=ORIENTED_EDGE('',*,*,#4907,.F.);
#7074=ORIENTED_EDGE('',*,*,#4908,.F.);
#7075=ORIENTED_EDGE('',*,*,#4907,.T.);
#7076=ORIENTED_EDGE('',*,*,#4904,.T.);
#7077=ORIENTED_EDGE('',*,*,#4909,.T.);
#7078=ORIENTED_EDGE('',*,*,#4910,.F.);
#7079=ORIENTED_EDGE('',*,*,#4911,.F.);
#7080=ORIENTED_EDGE('',*,*,#4912,.F.);
#7081=ORIENTED_EDGE('',*,*,#4911,.T.);
#7082=ORIENTED_EDGE('',*,*,#4913,.T.);
#7083=ORIENTED_EDGE('',*,*,#4914,.F.);
#7084=ORIENTED_EDGE('',*,*,#4913,.F.);
#7085=ORIENTED_EDGE('',*,*,#4910,.T.);
#7086=ORIENTED_EDGE('',*,*,#4915,.T.);
#7087=ORIENTED_EDGE('',*,*,#4916,.F.);
#7088=ORIENTED_EDGE('',*,*,#4917,.F.);
#7089=ORIENTED_EDGE('',*,*,#4918,.F.);
#7090=ORIENTED_EDGE('',*,*,#4917,.T.);
#7091=ORIENTED_EDGE('',*,*,#4919,.F.);
#7092=ORIENTED_EDGE('',*,*,#4920,.F.);
#7093=ORIENTED_EDGE('',*,*,#4919,.T.);
#7094=ORIENTED_EDGE('',*,*,#4916,.T.);
#7095=ORIENTED_EDGE('',*,*,#4921,.T.);
#7096=ORIENTED_EDGE('',*,*,#4922,.F.);
#7097=ORIENTED_EDGE('',*,*,#4923,.F.);
#7098=ORIENTED_EDGE('',*,*,#4924,.F.);
#7099=ORIENTED_EDGE('',*,*,#4923,.T.);
#7100=ORIENTED_EDGE('',*,*,#4925,.T.);
#7101=ORIENTED_EDGE('',*,*,#4926,.F.);
#7102=ORIENTED_EDGE('',*,*,#4927,.F.);
#7103=ORIENTED_EDGE('',*,*,#4928,.T.);
#7104=ORIENTED_EDGE('',*,*,#4929,.T.);
#7105=ORIENTED_EDGE('',*,*,#4930,.F.);
#7106=ORIENTED_EDGE('',*,*,#4931,.F.);
#7107=ORIENTED_EDGE('',*,*,#4932,.F.);
#7108=ORIENTED_EDGE('',*,*,#4931,.T.);
#7109=ORIENTED_EDGE('',*,*,#4933,.F.);
#7110=ORIENTED_EDGE('',*,*,#4934,.F.);
#7111=ORIENTED_EDGE('',*,*,#4925,.F.);
#7112=ORIENTED_EDGE('',*,*,#4922,.T.);
#7113=ORIENTED_EDGE('',*,*,#4935,.T.);
#7114=ORIENTED_EDGE('',*,*,#4936,.F.);
#7115=ORIENTED_EDGE('',*,*,#4937,.F.);
#7116=ORIENTED_EDGE('',*,*,#4938,.F.);
#7117=ORIENTED_EDGE('',*,*,#4937,.T.);
#7118=ORIENTED_EDGE('',*,*,#4939,.F.);
#7119=ORIENTED_EDGE('',*,*,#4940,.F.);
#7120=ORIENTED_EDGE('',*,*,#4941,.T.);
#7121=ORIENTED_EDGE('',*,*,#4901,.T.);
#7122=ORIENTED_EDGE('',*,*,#4942,.F.);
#7123=ORIENTED_EDGE('',*,*,#4933,.T.);
#7124=ORIENTED_EDGE('',*,*,#4930,.T.);
#7125=ORIENTED_EDGE('',*,*,#4943,.T.);
#7126=ORIENTED_EDGE('',*,*,#4902,.F.);
#7127=ORIENTED_EDGE('',*,*,#4941,.F.);
#7128=ORIENTED_EDGE('',*,*,#4944,.F.);
#7129=ORIENTED_EDGE('',*,*,#4945,.F.);
#7130=ORIENTED_EDGE('',*,*,#4946,.T.);
#7131=ORIENTED_EDGE('',*,*,#4927,.T.);
#7132=ORIENTED_EDGE('',*,*,#4947,.F.);
#7133=ORIENTED_EDGE('',*,*,#4939,.T.);
#7134=ORIENTED_EDGE('',*,*,#4936,.T.);
#7135=ORIENTED_EDGE('',*,*,#4948,.T.);
#7136=ORIENTED_EDGE('',*,*,#4928,.F.);
#7137=ORIENTED_EDGE('',*,*,#4946,.F.);
#7138=ORIENTED_EDGE('',*,*,#4909,.F.);
#7139=ORIENTED_EDGE('',*,*,#4903,.F.);
#7140=ORIENTED_EDGE('',*,*,#4943,.F.);
#7141=ORIENTED_EDGE('',*,*,#4929,.F.);
#7142=ORIENTED_EDGE('',*,*,#4948,.F.);
#7143=ORIENTED_EDGE('',*,*,#4935,.F.);
#7144=ORIENTED_EDGE('',*,*,#4921,.F.);
#7145=ORIENTED_EDGE('',*,*,#4915,.F.);
#7146=ORIENTED_EDGE('',*,*,#4949,.T.);
#7147=ORIENTED_EDGE('',*,*,#4950,.T.);
#7148=ORIENTED_EDGE('',*,*,#4951,.T.);
#7149=ORIENTED_EDGE('',*,*,#4950,.F.);
#7150=ORIENTED_EDGE('',*,*,#4952,.T.);
#7151=ORIENTED_EDGE('',*,*,#4949,.F.);
#7152=ORIENTED_EDGE('',*,*,#4953,.F.);
#7153=ORIENTED_EDGE('',*,*,#4954,.T.);
#7154=ORIENTED_EDGE('',*,*,#4951,.F.);
#7155=ORIENTED_EDGE('',*,*,#4954,.F.);
#7156=ORIENTED_EDGE('',*,*,#4955,.F.);
#7157=ORIENTED_EDGE('',*,*,#4956,.T.);
#7158=ORIENTED_EDGE('',*,*,#4953,.T.);
#7159=ORIENTED_EDGE('',*,*,#4956,.F.);
#7160=ORIENTED_EDGE('',*,*,#4957,.F.);
#7161=ORIENTED_EDGE('',*,*,#4958,.T.);
#7162=ORIENTED_EDGE('',*,*,#4955,.T.);
#7163=ORIENTED_EDGE('',*,*,#4958,.F.);
#7164=ORIENTED_EDGE('',*,*,#4957,.T.);
#7165=ORIENTED_EDGE('',*,*,#4934,.T.);
#7166=ORIENTED_EDGE('',*,*,#4938,.T.);
#7167=ORIENTED_EDGE('',*,*,#4947,.T.);
#7168=ORIENTED_EDGE('',*,*,#4945,.T.);
#7169=ORIENTED_EDGE('',*,*,#4926,.T.);
#7170=ORIENTED_EDGE('',*,*,#4932,.T.);
#7171=ORIENTED_EDGE('',*,*,#4942,.T.);
#7172=ORIENTED_EDGE('',*,*,#4959,.T.);
#7173=ORIENTED_EDGE('',*,*,#4960,.F.);
#7174=ORIENTED_EDGE('',*,*,#4961,.F.);
#7175=ORIENTED_EDGE('',*,*,#4959,.F.);
#7176=ORIENTED_EDGE('',*,*,#4944,.T.);
#7177=ORIENTED_EDGE('',*,*,#4940,.T.);
#7178=ORIENTED_EDGE('',*,*,#4900,.T.);
#7179=ORIENTED_EDGE('',*,*,#4906,.T.);
#7180=ORIENTED_EDGE('',*,*,#4908,.T.);
#7181=ORIENTED_EDGE('',*,*,#4912,.T.);
#7182=ORIENTED_EDGE('',*,*,#4914,.T.);
#7183=ORIENTED_EDGE('',*,*,#4918,.T.);
#7184=ORIENTED_EDGE('',*,*,#4920,.T.);
#7185=ORIENTED_EDGE('',*,*,#4924,.T.);
#7186=ORIENTED_EDGE('',*,*,#4952,.F.);
#7187=ORIENTED_EDGE('',*,*,#4962,.T.);
#7188=ORIENTED_EDGE('',*,*,#4960,.T.);
#7189=ORIENTED_EDGE('',*,*,#4961,.T.);
#7190=ORIENTED_EDGE('',*,*,#4962,.F.);
#7191=ORIENTED_EDGE('',*,*,#4963,.F.);
#7192=ORIENTED_EDGE('',*,*,#4964,.F.);
#7193=ORIENTED_EDGE('',*,*,#4965,.T.);
#7194=ORIENTED_EDGE('',*,*,#4966,.T.);
#7195=ORIENTED_EDGE('',*,*,#4967,.F.);
#7196=ORIENTED_EDGE('',*,*,#4968,.F.);
#7197=ORIENTED_EDGE('',*,*,#4969,.F.);
#7198=ORIENTED_EDGE('',*,*,#4968,.T.);
#7199=ORIENTED_EDGE('',*,*,#4970,.F.);
#7200=ORIENTED_EDGE('',*,*,#4971,.F.);
#7201=ORIENTED_EDGE('',*,*,#4970,.T.);
#7202=ORIENTED_EDGE('',*,*,#4967,.T.);
#7203=ORIENTED_EDGE('',*,*,#4972,.T.);
#7204=ORIENTED_EDGE('',*,*,#4973,.F.);
#7205=ORIENTED_EDGE('',*,*,#4974,.F.);
#7206=ORIENTED_EDGE('',*,*,#4975,.F.);
#7207=ORIENTED_EDGE('',*,*,#4974,.T.);
#7208=ORIENTED_EDGE('',*,*,#4976,.T.);
#7209=ORIENTED_EDGE('',*,*,#4977,.F.);
#7210=ORIENTED_EDGE('',*,*,#4976,.F.);
#7211=ORIENTED_EDGE('',*,*,#4973,.T.);
#7212=ORIENTED_EDGE('',*,*,#4978,.T.);
#7213=ORIENTED_EDGE('',*,*,#4979,.F.);
#7214=ORIENTED_EDGE('',*,*,#4980,.F.);
#7215=ORIENTED_EDGE('',*,*,#4981,.F.);
#7216=ORIENTED_EDGE('',*,*,#4980,.T.);
#7217=ORIENTED_EDGE('',*,*,#4982,.F.);
#7218=ORIENTED_EDGE('',*,*,#4983,.F.);
#7219=ORIENTED_EDGE('',*,*,#4982,.T.);
#7220=ORIENTED_EDGE('',*,*,#4979,.T.);
#7221=ORIENTED_EDGE('',*,*,#4984,.T.);
#7222=ORIENTED_EDGE('',*,*,#4985,.F.);
#7223=ORIENTED_EDGE('',*,*,#4986,.F.);
#7224=ORIENTED_EDGE('',*,*,#4987,.F.);
#7225=ORIENTED_EDGE('',*,*,#4986,.T.);
#7226=ORIENTED_EDGE('',*,*,#4988,.T.);
#7227=ORIENTED_EDGE('',*,*,#4989,.F.);
#7228=ORIENTED_EDGE('',*,*,#4990,.F.);
#7229=ORIENTED_EDGE('',*,*,#4991,.T.);
#7230=ORIENTED_EDGE('',*,*,#4992,.T.);
#7231=ORIENTED_EDGE('',*,*,#4993,.F.);
#7232=ORIENTED_EDGE('',*,*,#4994,.F.);
#7233=ORIENTED_EDGE('',*,*,#4995,.F.);
#7234=ORIENTED_EDGE('',*,*,#4994,.T.);
#7235=ORIENTED_EDGE('',*,*,#4996,.F.);
#7236=ORIENTED_EDGE('',*,*,#4997,.F.);
#7237=ORIENTED_EDGE('',*,*,#4988,.F.);
#7238=ORIENTED_EDGE('',*,*,#4985,.T.);
#7239=ORIENTED_EDGE('',*,*,#4998,.T.);
#7240=ORIENTED_EDGE('',*,*,#4999,.F.);
#7241=ORIENTED_EDGE('',*,*,#5000,.F.);
#7242=ORIENTED_EDGE('',*,*,#5001,.F.);
#7243=ORIENTED_EDGE('',*,*,#5000,.T.);
#7244=ORIENTED_EDGE('',*,*,#5002,.F.);
#7245=ORIENTED_EDGE('',*,*,#5003,.F.);
#7246=ORIENTED_EDGE('',*,*,#5004,.T.);
#7247=ORIENTED_EDGE('',*,*,#4964,.T.);
#7248=ORIENTED_EDGE('',*,*,#5005,.F.);
#7249=ORIENTED_EDGE('',*,*,#4996,.T.);
#7250=ORIENTED_EDGE('',*,*,#4993,.T.);
#7251=ORIENTED_EDGE('',*,*,#5006,.T.);
#7252=ORIENTED_EDGE('',*,*,#4965,.F.);
#7253=ORIENTED_EDGE('',*,*,#5004,.F.);
#7254=ORIENTED_EDGE('',*,*,#5007,.F.);
#7255=ORIENTED_EDGE('',*,*,#5008,.F.);
#7256=ORIENTED_EDGE('',*,*,#5009,.T.);
#7257=ORIENTED_EDGE('',*,*,#4990,.T.);
#7258=ORIENTED_EDGE('',*,*,#5010,.F.);
#7259=ORIENTED_EDGE('',*,*,#5002,.T.);
#7260=ORIENTED_EDGE('',*,*,#4999,.T.);
#7261=ORIENTED_EDGE('',*,*,#5011,.T.);
#7262=ORIENTED_EDGE('',*,*,#4991,.F.);
#7263=ORIENTED_EDGE('',*,*,#5009,.F.);
#7264=ORIENTED_EDGE('',*,*,#4972,.F.);
#7265=ORIENTED_EDGE('',*,*,#4966,.F.);
#7266=ORIENTED_EDGE('',*,*,#5006,.F.);
#7267=ORIENTED_EDGE('',*,*,#4992,.F.);
#7268=ORIENTED_EDGE('',*,*,#5011,.F.);
#7269=ORIENTED_EDGE('',*,*,#4998,.F.);
#7270=ORIENTED_EDGE('',*,*,#4984,.F.);
#7271=ORIENTED_EDGE('',*,*,#4978,.F.);
#7272=ORIENTED_EDGE('',*,*,#5012,.T.);
#7273=ORIENTED_EDGE('',*,*,#5013,.T.);
#7274=ORIENTED_EDGE('',*,*,#5014,.T.);
#7275=ORIENTED_EDGE('',*,*,#5013,.F.);
#7276=ORIENTED_EDGE('',*,*,#5015,.T.);
#7277=ORIENTED_EDGE('',*,*,#5012,.F.);
#7278=ORIENTED_EDGE('',*,*,#5016,.F.);
#7279=ORIENTED_EDGE('',*,*,#5017,.T.);
#7280=ORIENTED_EDGE('',*,*,#5014,.F.);
#7281=ORIENTED_EDGE('',*,*,#5017,.F.);
#7282=ORIENTED_EDGE('',*,*,#5018,.F.);
#7283=ORIENTED_EDGE('',*,*,#5019,.T.);
#7284=ORIENTED_EDGE('',*,*,#5016,.T.);
#7285=ORIENTED_EDGE('',*,*,#5019,.F.);
#7286=ORIENTED_EDGE('',*,*,#5020,.F.);
#7287=ORIENTED_EDGE('',*,*,#5021,.T.);
#7288=ORIENTED_EDGE('',*,*,#5018,.T.);
#7289=ORIENTED_EDGE('',*,*,#5021,.F.);
#7290=ORIENTED_EDGE('',*,*,#5020,.T.);
#7291=ORIENTED_EDGE('',*,*,#4997,.T.);
#7292=ORIENTED_EDGE('',*,*,#5001,.T.);
#7293=ORIENTED_EDGE('',*,*,#5010,.T.);
#7294=ORIENTED_EDGE('',*,*,#5008,.T.);
#7295=ORIENTED_EDGE('',*,*,#4989,.T.);
#7296=ORIENTED_EDGE('',*,*,#4995,.T.);
#7297=ORIENTED_EDGE('',*,*,#5005,.T.);
#7298=ORIENTED_EDGE('',*,*,#5022,.T.);
#7299=ORIENTED_EDGE('',*,*,#5023,.F.);
#7300=ORIENTED_EDGE('',*,*,#5024,.F.);
#7301=ORIENTED_EDGE('',*,*,#5022,.F.);
#7302=ORIENTED_EDGE('',*,*,#5007,.T.);
#7303=ORIENTED_EDGE('',*,*,#5003,.T.);
#7304=ORIENTED_EDGE('',*,*,#4963,.T.);
#7305=ORIENTED_EDGE('',*,*,#4969,.T.);
#7306=ORIENTED_EDGE('',*,*,#4971,.T.);
#7307=ORIENTED_EDGE('',*,*,#4975,.T.);
#7308=ORIENTED_EDGE('',*,*,#4977,.T.);
#7309=ORIENTED_EDGE('',*,*,#4981,.T.);
#7310=ORIENTED_EDGE('',*,*,#4983,.T.);
#7311=ORIENTED_EDGE('',*,*,#4987,.T.);
#7312=ORIENTED_EDGE('',*,*,#5015,.F.);
#7313=ORIENTED_EDGE('',*,*,#5025,.T.);
#7314=ORIENTED_EDGE('',*,*,#5023,.T.);
#7315=ORIENTED_EDGE('',*,*,#5024,.T.);
#7316=ORIENTED_EDGE('',*,*,#5025,.F.);
#7317=ORIENTED_EDGE('',*,*,#5026,.F.);
#7318=ORIENTED_EDGE('',*,*,#5027,.F.);
#7319=ORIENTED_EDGE('',*,*,#5028,.T.);
#7320=ORIENTED_EDGE('',*,*,#5029,.T.);
#7321=ORIENTED_EDGE('',*,*,#5030,.F.);
#7322=ORIENTED_EDGE('',*,*,#5031,.F.);
#7323=ORIENTED_EDGE('',*,*,#5032,.F.);
#7324=ORIENTED_EDGE('',*,*,#5031,.T.);
#7325=ORIENTED_EDGE('',*,*,#5033,.F.);
#7326=ORIENTED_EDGE('',*,*,#5034,.F.);
#7327=ORIENTED_EDGE('',*,*,#5033,.T.);
#7328=ORIENTED_EDGE('',*,*,#5030,.T.);
#7329=ORIENTED_EDGE('',*,*,#5035,.T.);
#7330=ORIENTED_EDGE('',*,*,#5036,.F.);
#7331=ORIENTED_EDGE('',*,*,#5037,.F.);
#7332=ORIENTED_EDGE('',*,*,#5038,.F.);
#7333=ORIENTED_EDGE('',*,*,#5037,.T.);
#7334=ORIENTED_EDGE('',*,*,#5039,.T.);
#7335=ORIENTED_EDGE('',*,*,#5040,.F.);
#7336=ORIENTED_EDGE('',*,*,#5039,.F.);
#7337=ORIENTED_EDGE('',*,*,#5036,.T.);
#7338=ORIENTED_EDGE('',*,*,#5041,.T.);
#7339=ORIENTED_EDGE('',*,*,#5042,.F.);
#7340=ORIENTED_EDGE('',*,*,#5043,.F.);
#7341=ORIENTED_EDGE('',*,*,#5044,.F.);
#7342=ORIENTED_EDGE('',*,*,#5043,.T.);
#7343=ORIENTED_EDGE('',*,*,#5045,.F.);
#7344=ORIENTED_EDGE('',*,*,#5046,.F.);
#7345=ORIENTED_EDGE('',*,*,#5045,.T.);
#7346=ORIENTED_EDGE('',*,*,#5042,.T.);
#7347=ORIENTED_EDGE('',*,*,#5047,.T.);
#7348=ORIENTED_EDGE('',*,*,#5048,.F.);
#7349=ORIENTED_EDGE('',*,*,#5049,.F.);
#7350=ORIENTED_EDGE('',*,*,#5050,.F.);
#7351=ORIENTED_EDGE('',*,*,#5049,.T.);
#7352=ORIENTED_EDGE('',*,*,#5051,.T.);
#7353=ORIENTED_EDGE('',*,*,#5052,.F.);
#7354=ORIENTED_EDGE('',*,*,#5053,.F.);
#7355=ORIENTED_EDGE('',*,*,#5054,.T.);
#7356=ORIENTED_EDGE('',*,*,#5055,.T.);
#7357=ORIENTED_EDGE('',*,*,#5056,.F.);
#7358=ORIENTED_EDGE('',*,*,#5057,.F.);
#7359=ORIENTED_EDGE('',*,*,#5058,.F.);
#7360=ORIENTED_EDGE('',*,*,#5057,.T.);
#7361=ORIENTED_EDGE('',*,*,#5059,.F.);
#7362=ORIENTED_EDGE('',*,*,#5060,.F.);
#7363=ORIENTED_EDGE('',*,*,#5051,.F.);
#7364=ORIENTED_EDGE('',*,*,#5048,.T.);
#7365=ORIENTED_EDGE('',*,*,#5061,.T.);
#7366=ORIENTED_EDGE('',*,*,#5062,.F.);
#7367=ORIENTED_EDGE('',*,*,#5063,.F.);
#7368=ORIENTED_EDGE('',*,*,#5064,.F.);
#7369=ORIENTED_EDGE('',*,*,#5063,.T.);
#7370=ORIENTED_EDGE('',*,*,#5065,.F.);
#7371=ORIENTED_EDGE('',*,*,#5066,.F.);
#7372=ORIENTED_EDGE('',*,*,#5067,.T.);
#7373=ORIENTED_EDGE('',*,*,#5027,.T.);
#7374=ORIENTED_EDGE('',*,*,#5068,.F.);
#7375=ORIENTED_EDGE('',*,*,#5059,.T.);
#7376=ORIENTED_EDGE('',*,*,#5056,.T.);
#7377=ORIENTED_EDGE('',*,*,#5069,.T.);
#7378=ORIENTED_EDGE('',*,*,#5028,.F.);
#7379=ORIENTED_EDGE('',*,*,#5067,.F.);
#7380=ORIENTED_EDGE('',*,*,#5070,.F.);
#7381=ORIENTED_EDGE('',*,*,#5071,.F.);
#7382=ORIENTED_EDGE('',*,*,#5072,.T.);
#7383=ORIENTED_EDGE('',*,*,#5053,.T.);
#7384=ORIENTED_EDGE('',*,*,#5073,.F.);
#7385=ORIENTED_EDGE('',*,*,#5065,.T.);
#7386=ORIENTED_EDGE('',*,*,#5062,.T.);
#7387=ORIENTED_EDGE('',*,*,#5074,.T.);
#7388=ORIENTED_EDGE('',*,*,#5054,.F.);
#7389=ORIENTED_EDGE('',*,*,#5072,.F.);
#7390=ORIENTED_EDGE('',*,*,#5035,.F.);
#7391=ORIENTED_EDGE('',*,*,#5029,.F.);
#7392=ORIENTED_EDGE('',*,*,#5069,.F.);
#7393=ORIENTED_EDGE('',*,*,#5055,.F.);
#7394=ORIENTED_EDGE('',*,*,#5074,.F.);
#7395=ORIENTED_EDGE('',*,*,#5061,.F.);
#7396=ORIENTED_EDGE('',*,*,#5047,.F.);
#7397=ORIENTED_EDGE('',*,*,#5041,.F.);
#7398=ORIENTED_EDGE('',*,*,#5075,.T.);
#7399=ORIENTED_EDGE('',*,*,#5076,.T.);
#7400=ORIENTED_EDGE('',*,*,#5077,.T.);
#7401=ORIENTED_EDGE('',*,*,#5076,.F.);
#7402=ORIENTED_EDGE('',*,*,#5078,.T.);
#7403=ORIENTED_EDGE('',*,*,#5075,.F.);
#7404=ORIENTED_EDGE('',*,*,#5079,.F.);
#7405=ORIENTED_EDGE('',*,*,#5080,.T.);
#7406=ORIENTED_EDGE('',*,*,#5077,.F.);
#7407=ORIENTED_EDGE('',*,*,#5080,.F.);
#7408=ORIENTED_EDGE('',*,*,#5081,.F.);
#7409=ORIENTED_EDGE('',*,*,#5082,.T.);
#7410=ORIENTED_EDGE('',*,*,#5079,.T.);
#7411=ORIENTED_EDGE('',*,*,#5082,.F.);
#7412=ORIENTED_EDGE('',*,*,#5083,.F.);
#7413=ORIENTED_EDGE('',*,*,#5084,.T.);
#7414=ORIENTED_EDGE('',*,*,#5081,.T.);
#7415=ORIENTED_EDGE('',*,*,#5084,.F.);
#7416=ORIENTED_EDGE('',*,*,#5083,.T.);
#7417=ORIENTED_EDGE('',*,*,#5060,.T.);
#7418=ORIENTED_EDGE('',*,*,#5064,.T.);
#7419=ORIENTED_EDGE('',*,*,#5073,.T.);
#7420=ORIENTED_EDGE('',*,*,#5071,.T.);
#7421=ORIENTED_EDGE('',*,*,#5052,.T.);
#7422=ORIENTED_EDGE('',*,*,#5058,.T.);
#7423=ORIENTED_EDGE('',*,*,#5068,.T.);
#7424=ORIENTED_EDGE('',*,*,#5085,.T.);
#7425=ORIENTED_EDGE('',*,*,#5086,.F.);
#7426=ORIENTED_EDGE('',*,*,#5087,.F.);
#7427=ORIENTED_EDGE('',*,*,#5085,.F.);
#7428=ORIENTED_EDGE('',*,*,#5070,.T.);
#7429=ORIENTED_EDGE('',*,*,#5066,.T.);
#7430=ORIENTED_EDGE('',*,*,#5026,.T.);
#7431=ORIENTED_EDGE('',*,*,#5032,.T.);
#7432=ORIENTED_EDGE('',*,*,#5034,.T.);
#7433=ORIENTED_EDGE('',*,*,#5038,.T.);
#7434=ORIENTED_EDGE('',*,*,#5040,.T.);
#7435=ORIENTED_EDGE('',*,*,#5044,.T.);
#7436=ORIENTED_EDGE('',*,*,#5046,.T.);
#7437=ORIENTED_EDGE('',*,*,#5050,.T.);
#7438=ORIENTED_EDGE('',*,*,#5078,.F.);
#7439=ORIENTED_EDGE('',*,*,#5088,.T.);
#7440=ORIENTED_EDGE('',*,*,#5086,.T.);
#7441=ORIENTED_EDGE('',*,*,#5087,.T.);
#7442=ORIENTED_EDGE('',*,*,#5088,.F.);
#7443=CYLINDRICAL_SURFACE('',#8262,4.5);
#7444=CYLINDRICAL_SURFACE('',#8268,1.);
#7445=CYLINDRICAL_SURFACE('',#8271,0.999999999999998);
#7446=CYLINDRICAL_SURFACE('',#8284,1.);
#7447=CYLINDRICAL_SURFACE('',#8287,1.);
#7448=CYLINDRICAL_SURFACE('',#8290,1.);
#7449=CYLINDRICAL_SURFACE('',#8292,1.);
#7450=CYLINDRICAL_SURFACE('',#8299,1.);
#7451=CYLINDRICAL_SURFACE('',#8304,1.);
#7452=CYLINDRICAL_SURFACE('',#8308,1.);
#7453=CYLINDRICAL_SURFACE('',#8314,1.);
#7454=CYLINDRICAL_SURFACE('',#8322,1.);
#7455=CYLINDRICAL_SURFACE('',#8327,2.);
#7456=CYLINDRICAL_SURFACE('',#8331,2.);
#7457=CYLINDRICAL_SURFACE('',#8343,1.5);
#7458=CYLINDRICAL_SURFACE('',#8347,1.5);
#7459=CYLINDRICAL_SURFACE('',#8351,1.5);
#7460=CYLINDRICAL_SURFACE('',#8354,1.5);
#7461=CYLINDRICAL_SURFACE('',#8371,3.);
#7462=CYLINDRICAL_SURFACE('',#8373,4.5);
#7463=CYLINDRICAL_SURFACE('',#8379,4.5);
#7464=CYLINDRICAL_SURFACE('',#8382,4.5);
#7465=CYLINDRICAL_SURFACE('',#8386,1.);
#7466=CYLINDRICAL_SURFACE('',#8392,1.);
#7467=CYLINDRICAL_SURFACE('',#8398,1.);
#7468=CYLINDRICAL_SURFACE('',#8402,1.);
#7469=CYLINDRICAL_SURFACE('',#8406,1.);
#7470=CYLINDRICAL_SURFACE('',#8408,1.);
#7471=CYLINDRICAL_SURFACE('',#8422,1.);
#7472=CYLINDRICAL_SURFACE('',#8425,2.5);
#7473=CYLINDRICAL_SURFACE('',#8428,1.);
#7474=CYLINDRICAL_SURFACE('',#8430,2.);
#7475=CYLINDRICAL_SURFACE('',#8431,2.);
#7476=CYLINDRICAL_SURFACE('',#8433,0.999999999999996);
#7477=CYLINDRICAL_SURFACE('',#8435,1.);
#7478=CYLINDRICAL_SURFACE('',#8437,2.5);
#7479=CYLINDRICAL_SURFACE('',#8440,1.);
#7480=CYLINDRICAL_SURFACE('',#8444,2.5);
#7481=CYLINDRICAL_SURFACE('',#8451,2.5);
#7482=CYLINDRICAL_SURFACE('',#8459,2.);
#7483=CYLINDRICAL_SURFACE('',#8460,2.);
#7484=CYLINDRICAL_SURFACE('',#8461,2.);
#7485=CYLINDRICAL_SURFACE('',#8477,1.);
#7486=CYLINDRICAL_SURFACE('',#8483,1.);
#7487=CYLINDRICAL_SURFACE('',#8485,1.);
#7488=CYLINDRICAL_SURFACE('',#8489,2.);
#7489=CYLINDRICAL_SURFACE('',#8492,2.);
#7490=CYLINDRICAL_SURFACE('',#8497,1.);
#7491=CYLINDRICAL_SURFACE('',#8498,2.);
#7492=CYLINDRICAL_SURFACE('',#8504,4.);
#7493=CYLINDRICAL_SURFACE('',#8509,0.999999999999999);
#7494=CYLINDRICAL_SURFACE('',#8511,1.);
#7495=CYLINDRICAL_SURFACE('',#8520,2.);
#7496=CYLINDRICAL_SURFACE('',#8525,2.);
#7497=CYLINDRICAL_SURFACE('',#8540,3.);
#7498=CYLINDRICAL_SURFACE('',#8542,3.5);
#7499=CYLINDRICAL_SURFACE('',#8543,3.5);
#7500=CYLINDRICAL_SURFACE('',#8544,3.5);
#7501=CYLINDRICAL_SURFACE('',#8545,3.5);
#7502=CYLINDRICAL_SURFACE('',#8547,1.5);
#7503=CYLINDRICAL_SURFACE('',#8550,1.5);
#7504=CYLINDRICAL_SURFACE('',#8553,1.5);
#7505=CYLINDRICAL_SURFACE('',#8556,1.5);
#7506=CYLINDRICAL_SURFACE('',#8559,1.);
#7507=CYLINDRICAL_SURFACE('',#8566,1.);
#7508=CYLINDRICAL_SURFACE('',#8571,1.);
#7509=CYLINDRICAL_SURFACE('',#8576,1.);
#7510=CYLINDRICAL_SURFACE('',#8581,1.);
#7511=CYLINDRICAL_SURFACE('',#8586,1.);
#7512=CYLINDRICAL_SURFACE('',#8590,2.);
#7513=CYLINDRICAL_SURFACE('',#8592,1.99999999999999);
#7514=CYLINDRICAL_SURFACE('',#8594,0.999999999999996);
#7515=CYLINDRICAL_SURFACE('',#8597,2.00000000000001);
#7516=CYLINDRICAL_SURFACE('',#8598,2.);
#7517=CYLINDRICAL_SURFACE('',#8600,2.);
#7518=CYLINDRICAL_SURFACE('',#8602,3.20000000000001);
#7519=CYLINDRICAL_SURFACE('',#8605,3.20000000000001);
#7520=CYLINDRICAL_SURFACE('',#8608,3.2);
#7521=CYLINDRICAL_SURFACE('',#8611,3.2);
#7522=CYLINDRICAL_SURFACE('',#8624,0.999999999999999);
#7523=CYLINDRICAL_SURFACE('',#8627,0.999999999999999);
#7524=CYLINDRICAL_SURFACE('',#8630,1.);
#7525=CYLINDRICAL_SURFACE('',#8633,0.999999999999999);
#7526=CYLINDRICAL_SURFACE('',#8636,2.);
#7527=CYLINDRICAL_SURFACE('',#8639,2.);
#7528=CYLINDRICAL_SURFACE('',#8642,2.);
#7529=CYLINDRICAL_SURFACE('',#8645,2.);
#7530=CYLINDRICAL_SURFACE('',#8649,2.);
#7531=CYLINDRICAL_SURFACE('',#8652,2.);
#7532=CYLINDRICAL_SURFACE('',#8657,2.);
#7533=CYLINDRICAL_SURFACE('',#8662,2.);
#7534=CYLINDRICAL_SURFACE('',#8669,2.);
#7535=CYLINDRICAL_SURFACE('',#8672,2.00000000000001);
#7536=CYLINDRICAL_SURFACE('',#8681,0.2);
#7537=CYLINDRICAL_SURFACE('',#8688,0.2);
#7538=CYLINDRICAL_SURFACE('',#8694,0.999999999999871);
#7539=CYLINDRICAL_SURFACE('',#8697,0.999999999999871);
#7540=CYLINDRICAL_SURFACE('',#8700,0.2);
#7541=CYLINDRICAL_SURFACE('',#8711,0.2);
#7542=CYLINDRICAL_SURFACE('',#8718,0.2);
#7543=CYLINDRICAL_SURFACE('',#8723,0.999999999999871);
#7544=CYLINDRICAL_SURFACE('',#8726,0.999999999999871);
#7545=CYLINDRICAL_SURFACE('',#8729,0.2);
#7546=CYLINDRICAL_SURFACE('',#8734,0.2);
#7547=CYLINDRICAL_SURFACE('',#8739,0.2);
#7548=CYLINDRICAL_SURFACE('',#8743,0.4);
#7549=CYLINDRICAL_SURFACE('',#8745,9.);
#7550=CYLINDRICAL_SURFACE('',#8747,0.2);
#7551=CYLINDRICAL_SURFACE('',#8752,0.2);
#7552=CYLINDRICAL_SURFACE('',#8756,0.4);
#7553=CYLINDRICAL_SURFACE('',#8759,0.4);
#7554=CYLINDRICAL_SURFACE('',#8765,0.4);
#7555=CYLINDRICAL_SURFACE('',#8775,0.4);
#7556=CYLINDRICAL_SURFACE('',#8779,0.4);
#7557=CYLINDRICAL_SURFACE('',#8785,0.4);
#7558=CYLINDRICAL_SURFACE('',#8795,0.4);
#7559=CYLINDRICAL_SURFACE('',#8799,0.800000000000058);
#7560=CYLINDRICAL_SURFACE('',#8800,0.800000000000058);
#7561=CYLINDRICAL_SURFACE('',#8803,2.98575787723652);
#7562=CYLINDRICAL_SURFACE('',#8810,2.98575787723652);
#7563=CYLINDRICAL_SURFACE('',#8811,0.399999999999998);
#7564=CYLINDRICAL_SURFACE('',#8813,0.4);
#7565=CYLINDRICAL_SURFACE('',#8815,0.400000000000004);
#7566=CYLINDRICAL_SURFACE('',#8817,0.4);
#7567=CYLINDRICAL_SURFACE('',#8819,2.);
#7568=CYLINDRICAL_SURFACE('',#8822,2.);
#7569=CYLINDRICAL_SURFACE('',#8830,7.);
#7570=CYLINDRICAL_SURFACE('',#8838,9.);
#7571=CYLINDRICAL_SURFACE('',#8844,0.4);
#7572=CYLINDRICAL_SURFACE('',#8847,0.4);
#7573=CYLINDRICAL_SURFACE('',#8850,0.4);
#7574=CYLINDRICAL_SURFACE('',#8851,0.4);
#7575=CYLINDRICAL_SURFACE('',#8868,0.4);
#7576=CYLINDRICAL_SURFACE('',#8871,0.4);
#7577=CYLINDRICAL_SURFACE('',#8874,0.4);
#7578=CYLINDRICAL_SURFACE('',#8878,0.4);
#7579=CYLINDRICAL_SURFACE('',#8879,9.);
#7580=CYLINDRICAL_SURFACE('',#8894,7.);
#7581=CYLINDRICAL_SURFACE('',#8904,5.);
#7582=CYLINDRICAL_SURFACE('',#8906,4.);
#7583=CYLINDRICAL_SURFACE('',#8909,8.866);
#7584=CYLINDRICAL_SURFACE('',#8911,8.866);
#7585=CYLINDRICAL_SURFACE('',#8912,8.866);
#7586=CYLINDRICAL_SURFACE('',#8913,8.866);
#7587=CYLINDRICAL_SURFACE('',#8914,8.866);
#7588=CYLINDRICAL_SURFACE('',#8915,8.866);
#7589=CYLINDRICAL_SURFACE('',#8916,7.4455);
#7590=CYLINDRICAL_SURFACE('',#8918,7.4455);
#7591=CYLINDRICAL_SURFACE('',#8919,7.4455);
#7592=CYLINDRICAL_SURFACE('',#8920,7.4455);
#7593=CYLINDRICAL_SURFACE('',#8921,7.4455);
#7594=CYLINDRICAL_SURFACE('',#8922,7.4455);
#7595=CYLINDRICAL_SURFACE('',#8927,11.);
#7596=CYLINDRICAL_SURFACE('',#8933,7.);
#7597=CYLINDRICAL_SURFACE('',#8934,8.866);
#7598=CYLINDRICAL_SURFACE('',#8948,0.5);
#7599=CYLINDRICAL_SURFACE('',#8949,0.5);
#7600=CYLINDRICAL_SURFACE('',#8950,0.5);
#7601=CYLINDRICAL_SURFACE('',#8951,0.5);
#7602=CYLINDRICAL_SURFACE('',#8953,0.399999999999997);
#7603=CYLINDRICAL_SURFACE('',#8956,0.4);
#7604=CYLINDRICAL_SURFACE('',#8964,2.);
#7605=CYLINDRICAL_SURFACE('',#8968,2.);
#7606=CYLINDRICAL_SURFACE('',#8971,2.);
#7607=CYLINDRICAL_SURFACE('',#8975,2.);
#7608=CYLINDRICAL_SURFACE('',#8987,1.3);
#7609=CYLINDRICAL_SURFACE('',#8988,1.3);
#7610=CYLINDRICAL_SURFACE('',#8989,1.3);
#7611=CYLINDRICAL_SURFACE('',#8990,1.3);
#7612=CYLINDRICAL_SURFACE('',#8992,0.4);
#7613=CYLINDRICAL_SURFACE('',#8994,0.399999999999998);
#7614=CYLINDRICAL_SURFACE('',#8996,0.496);
#7615=CYLINDRICAL_SURFACE('',#9007,0.496);
#7616=CYLINDRICAL_SURFACE('',#9017,0.496);
#7617=CYLINDRICAL_SURFACE('',#9023,0.496);
#7618=CYLINDRICAL_SURFACE('',#9044,0.839230484541328);
#7619=CYLINDRICAL_SURFACE('',#9048,0.96675);
#7620=CYLINDRICAL_SURFACE('',#9057,0.496);
#7621=CYLINDRICAL_SURFACE('',#9068,0.496);
#7622=CYLINDRICAL_SURFACE('',#9078,0.496);
#7623=CYLINDRICAL_SURFACE('',#9084,0.496);
#7624=CYLINDRICAL_SURFACE('',#9105,0.839230484541328);
#7625=CYLINDRICAL_SURFACE('',#9109,0.96675);
#7626=CYLINDRICAL_SURFACE('',#9118,0.496);
#7627=CYLINDRICAL_SURFACE('',#9129,0.496);
#7628=CYLINDRICAL_SURFACE('',#9139,0.496);
#7629=CYLINDRICAL_SURFACE('',#9145,0.496);
#7630=CYLINDRICAL_SURFACE('',#9166,0.839230484541328);
#7631=CYLINDRICAL_SURFACE('',#9170,0.96675);
#7632=CYLINDRICAL_SURFACE('',#9179,0.496);
#7633=CYLINDRICAL_SURFACE('',#9190,0.496);
#7634=CYLINDRICAL_SURFACE('',#9200,0.496);
#7635=CYLINDRICAL_SURFACE('',#9206,0.496);
#7636=CYLINDRICAL_SURFACE('',#9227,0.839230484541328);
#7637=CYLINDRICAL_SURFACE('',#9231,0.96675);
#7638=ADVANCED_FACE('',(#476),#7443,.T.);
#7639=ADVANCED_FACE('',(#477),#284,.T.);
#7640=ADVANCED_FACE('',(#478),#285,.F.);
#7641=ADVANCED_FACE('',(#479),#7444,.F.);
#7642=ADVANCED_FACE('',(#480),#286,.F.);
#7643=ADVANCED_FACE('',(#481),#7445,.F.);
#7644=ADVANCED_FACE('',(#482),#287,.F.);
#7645=ADVANCED_FACE('',(#483),#288,.F.);
#7646=ADVANCED_FACE('',(#484),#289,.F.);
#7647=ADVANCED_FACE('',(#485),#290,.F.);
#7648=ADVANCED_FACE('',(#486),#7446,.T.);
#7649=ADVANCED_FACE('',(#487),#7447,.T.);
#7650=ADVANCED_FACE('',(#488),#7448,.T.);
#7651=ADVANCED_FACE('',(#489),#7449,.T.);
#7652=ADVANCED_FACE('',(#490),#214,.T.);
#7653=ADVANCED_FACE('',(#491),#7450,.T.);
#7654=ADVANCED_FACE('',(#492),#215,.T.);
#7655=ADVANCED_FACE('',(#493),#7451,.T.);
#7656=ADVANCED_FACE('',(#494),#196,.T.);
#7657=ADVANCED_FACE('',(#495),#7452,.T.);
#7658=ADVANCED_FACE('',(#496),#197,.T.);
#7659=ADVANCED_FACE('',(#497),#291,.T.);
#7660=ADVANCED_FACE('',(#498),#7453,.T.);
#7661=ADVANCED_FACE('',(#499),#292,.T.);
#7662=ADVANCED_FACE('',(#500),#7454,.T.);
#7663=ADVANCED_FACE('',(#501),#293,.T.);
#7664=ADVANCED_FACE('',(#502),#294,.F.);
#7665=ADVANCED_FACE('',(#503),#295,.F.);
#7666=ADVANCED_FACE('',(#504),#7455,.F.);
#7667=ADVANCED_FACE('',(#505),#296,.F.);
#7668=ADVANCED_FACE('',(#506),#7456,.F.);
#7669=ADVANCED_FACE('',(#507),#297,.T.);
#7670=ADVANCED_FACE('',(#508),#298,.F.);
#7671=ADVANCED_FACE('',(#509),#7457,.F.);
#7672=ADVANCED_FACE('',(#510),#7458,.F.);
#7673=ADVANCED_FACE('',(#511),#7459,.F.);
#7674=ADVANCED_FACE('',(#512),#7460,.F.);
#7675=ADVANCED_FACE('',(#513),#299,.F.);
#7676=ADVANCED_FACE('',(#514),#300,.F.);
#7677=ADVANCED_FACE('',(#515),#301,.F.);
#7678=ADVANCED_FACE('',(#516),#302,.F.);
#7679=ADVANCED_FACE('',(#517),#303,.F.);
#7680=ADVANCED_FACE('',(#518),#304,.T.);
#7681=ADVANCED_FACE('',(#519),#305,.F.);
#7682=ADVANCED_FACE('',(#520),#306,.F.);
#7683=ADVANCED_FACE('',(#521),#307,.F.);
#7684=ADVANCED_FACE('',(#522),#7461,.T.);
#7685=ADVANCED_FACE('',(#523),#7462,.T.);
#7686=ADVANCED_FACE('',(#524),#308,.T.);
#7687=ADVANCED_FACE('',(#525),#309,.T.);
#7688=ADVANCED_FACE('',(#526),#310,.F.);
#7689=ADVANCED_FACE('',(#527),#311,.F.);
#7690=ADVANCED_FACE('',(#528),#7463,.T.);
#7691=ADVANCED_FACE('',(#529),#312,.T.);
#7692=ADVANCED_FACE('',(#530),#313,.T.);
#7693=ADVANCED_FACE('',(#531),#7464,.T.);
#7694=ADVANCED_FACE('',(#532),#314,.F.);
#7695=ADVANCED_FACE('',(#533),#315,.T.);
#7696=ADVANCED_FACE('',(#534),#7465,.T.);
#7697=ADVANCED_FACE('',(#535),#216,.T.);
#7698=ADVANCED_FACE('',(#536),#7466,.T.);
#7699=ADVANCED_FACE('',(#537),#217,.T.);
#7700=ADVANCED_FACE('',(#538),#7467,.T.);
#7701=ADVANCED_FACE('',(#539),#178,.F.);
#7702=ADVANCED_FACE('',(#540),#7468,.T.);
#7703=ADVANCED_FACE('',(#541),#179,.F.);
#7704=ADVANCED_FACE('',(#542),#7469,.T.);
#7705=ADVANCED_FACE('',(#543),#7470,.T.);
#7706=ADVANCED_FACE('',(#544),#218,.T.);
#7707=ADVANCED_FACE('',(#545),#198,.T.);
#7708=ADVANCED_FACE('',(#546),#199,.T.);
#7709=ADVANCED_FACE('',(#547),#200,.T.);
#7710=ADVANCED_FACE('',(#548),#201,.T.);
#7711=ADVANCED_FACE('',(#549),#7471,.T.);
#7712=ADVANCED_FACE('',(#550),#316,.F.);
#7713=ADVANCED_FACE('',(#551),#7472,.F.);
#7714=ADVANCED_FACE('',(#552),#317,.F.);
#7715=ADVANCED_FACE('',(#553),#7473,.T.);
#7716=ADVANCED_FACE('',(#554),#7474,.T.);
#7717=ADVANCED_FACE('',(#555),#7475,.T.);
#7718=ADVANCED_FACE('',(#556),#318,.T.);
#7719=ADVANCED_FACE('',(#557),#7476,.F.);
#7720=ADVANCED_FACE('',(#558),#7477,.T.);
#7721=ADVANCED_FACE('',(#559),#7478,.F.);
#7722=ADVANCED_FACE('',(#560),#319,.F.);
#7723=ADVANCED_FACE('',(#561),#7479,.T.);
#7724=ADVANCED_FACE('',(#562),#320,.F.);
#7725=ADVANCED_FACE('',(#563),#321,.F.);
#7726=ADVANCED_FACE('',(#564),#7480,.F.);
#7727=ADVANCED_FACE('',(#565,#138),#322,.T.);
#7728=ADVANCED_FACE('',(#566,#139),#323,.T.);
#7729=ADVANCED_FACE('',(#567),#324,.F.);
#7730=ADVANCED_FACE('',(#568),#7481,.F.);
#7731=ADVANCED_FACE('',(#569),#325,.F.);
#7732=ADVANCED_FACE('',(#570,#140),#326,.T.);
#7733=ADVANCED_FACE('',(#571,#141),#327,.T.);
#7734=ADVANCED_FACE('',(#572),#328,.T.);
#7735=ADVANCED_FACE('',(#573),#329,.T.);
#7736=ADVANCED_FACE('',(#574),#7482,.T.);
#7737=ADVANCED_FACE('',(#575),#7483,.T.);
#7738=ADVANCED_FACE('',(#576),#7484,.T.);
#7739=ADVANCED_FACE('',(#577,#142,#143),#330,.F.);
#7740=ADVANCED_FACE('',(#578),#180,.F.);
#7741=ADVANCED_FACE('',(#579),#7485,.T.);
#7742=ADVANCED_FACE('',(#580),#181,.F.);
#7743=ADVANCED_FACE('',(#581),#7486,.T.);
#7744=ADVANCED_FACE('',(#582),#7487,.T.);
#7745=ADVANCED_FACE('',(#583),#182,.F.);
#7746=ADVANCED_FACE('',(#584),#7488,.T.);
#7747=ADVANCED_FACE('',(#585),#331,.T.);
#7748=ADVANCED_FACE('',(#586),#7489,.T.);
#7749=ADVANCED_FACE('',(#587,#144),#332,.T.);
#7750=ADVANCED_FACE('',(#588),#333,.F.);
#7751=ADVANCED_FACE('',(#589),#7490,.T.);
#7752=ADVANCED_FACE('',(#590),#7491,.T.);
#7753=ADVANCED_FACE('',(#591),#334,.T.);
#7754=ADVANCED_FACE('',(#592),#335,.T.);
#7755=ADVANCED_FACE('',(#593),#7492,.F.);
#7756=ADVANCED_FACE('',(#594,#145),#336,.T.);
#7757=ADVANCED_FACE('',(#595),#337,.F.);
#7758=ADVANCED_FACE('',(#596),#338,.F.);
#7759=ADVANCED_FACE('',(#597),#7493,.F.);
#7760=ADVANCED_FACE('',(#598),#7494,.F.);
#7761=ADVANCED_FACE('',(#599,#146,#147),#339,.F.);
#7762=ADVANCED_FACE('',(#600),#7495,.F.);
#7763=ADVANCED_FACE('',(#601),#340,.F.);
#7764=ADVANCED_FACE('',(#602),#341,.F.);
#7765=ADVANCED_FACE('',(#603),#7496,.F.);
#7766=ADVANCED_FACE('',(#604),#342,.F.);
#7767=ADVANCED_FACE('',(#605),#343,.T.);
#7768=ADVANCED_FACE('',(#606),#344,.F.);
#7769=ADVANCED_FACE('',(#607),#345,.F.);
#7770=ADVANCED_FACE('',(#608),#346,.F.);
#7771=ADVANCED_FACE('',(#609),#347,.F.);
#7772=ADVANCED_FACE('',(#610),#348,.F.);
#7773=ADVANCED_FACE('',(#611),#7497,.T.);
#7774=ADVANCED_FACE('',(#612),#349,.F.);
#7775=ADVANCED_FACE('',(#613),#7498,.T.);
#7776=ADVANCED_FACE('',(#614),#7499,.T.);
#7777=ADVANCED_FACE('',(#615),#7500,.T.);
#7778=ADVANCED_FACE('',(#616),#7501,.T.);
#7779=ADVANCED_FACE('',(#617),#350,.F.);
#7780=ADVANCED_FACE('',(#618),#7502,.F.);
#7781=ADVANCED_FACE('',(#619),#351,.T.);
#7782=ADVANCED_FACE('',(#620),#7503,.F.);
#7783=ADVANCED_FACE('',(#621),#352,.T.);
#7784=ADVANCED_FACE('',(#622),#7504,.F.);
#7785=ADVANCED_FACE('',(#623),#353,.T.);
#7786=ADVANCED_FACE('',(#624),#7505,.F.);
#7787=ADVANCED_FACE('',(#625),#354,.T.);
#7788=ADVANCED_FACE('',(#626),#7506,.T.);
#7789=ADVANCED_FACE('',(#627),#219,.T.);
#7790=ADVANCED_FACE('',(#628),#7507,.T.);
#7791=ADVANCED_FACE('',(#629),#183,.F.);
#7792=ADVANCED_FACE('',(#630),#7508,.T.);
#7793=ADVANCED_FACE('',(#631),#184,.F.);
#7794=ADVANCED_FACE('',(#632),#7509,.T.);
#7795=ADVANCED_FACE('',(#633),#185,.F.);
#7796=ADVANCED_FACE('',(#634),#7510,.T.);
#7797=ADVANCED_FACE('',(#635),#186,.F.);
#7798=ADVANCED_FACE('',(#636),#7511,.T.);
#7799=ADVANCED_FACE('',(#637),#187,.F.);
#7800=ADVANCED_FACE('',(#638),#7512,.T.);
#7801=ADVANCED_FACE('',(#639),#355,.T.);
#7802=ADVANCED_FACE('',(#640),#7513,.T.);
#7803=ADVANCED_FACE('',(#641),#356,.T.);
#7804=ADVANCED_FACE('',(#642),#7514,.F.);
#7805=ADVANCED_FACE('',(#643),#357,.T.);
#7806=ADVANCED_FACE('',(#644),#358,.T.);
#7807=ADVANCED_FACE('',(#645),#7515,.T.);
#7808=ADVANCED_FACE('',(#646),#7516,.T.);
#7809=ADVANCED_FACE('',(#647),#359,.T.);
#7810=ADVANCED_FACE('',(#648),#7517,.T.);
#7811=ADVANCED_FACE('',(#649),#7518,.F.);
#7812=ADVANCED_FACE('',(#650),#7519,.F.);
#7813=ADVANCED_FACE('',(#651),#7520,.F.);
#7814=ADVANCED_FACE('',(#652),#7521,.F.);
#7815=ADVANCED_FACE('',(#653,#148),#360,.F.);
#7816=ADVANCED_FACE('',(#654),#361,.T.);
#7817=ADVANCED_FACE('',(#655),#7522,.F.);
#7818=ADVANCED_FACE('',(#656,#149,#150),#362,.T.);
#7819=ADVANCED_FACE('',(#657),#7523,.F.);
#7820=ADVANCED_FACE('',(#658),#363,.T.);
#7821=ADVANCED_FACE('',(#659),#7524,.F.);
#7822=ADVANCED_FACE('',(#660,#151,#152),#364,.T.);
#7823=ADVANCED_FACE('',(#661),#7525,.F.);
#7824=ADVANCED_FACE('',(#662),#365,.T.);
#7825=ADVANCED_FACE('',(#663),#7526,.T.);
#7826=ADVANCED_FACE('',(#664,#153,#154),#366,.T.);
#7827=ADVANCED_FACE('',(#665),#7527,.T.);
#7828=ADVANCED_FACE('',(#666),#367,.T.);
#7829=ADVANCED_FACE('',(#667),#7528,.T.);
#7830=ADVANCED_FACE('',(#668,#155,#156),#368,.T.);
#7831=ADVANCED_FACE('',(#669),#7529,.T.);
#7832=ADVANCED_FACE('',(#670,#157),#369,.T.);
#7833=ADVANCED_FACE('',(#671),#7530,.T.);
#7834=ADVANCED_FACE('',(#672),#7531,.T.);
#7835=ADVANCED_FACE('',(#673),#202,.T.);
#7836=ADVANCED_FACE('',(#674),#7532,.T.);
#7837=ADVANCED_FACE('',(#675),#203,.T.);
#7838=ADVANCED_FACE('',(#676),#7533,.T.);
#7839=ADVANCED_FACE('',(#677),#204,.T.);
#7840=ADVANCED_FACE('',(#678),#205,.T.);
#7841=ADVANCED_FACE('',(#679),#7534,.T.);
#7842=ADVANCED_FACE('',(#680),#370,.T.);
#7843=ADVANCED_FACE('',(#681),#7535,.T.);
#7844=ADVANCED_FACE('',(#682),#371,.T.);
#7845=ADVANCED_FACE('',(#683,#158),#372,.T.);
#7846=ADVANCED_FACE('',(#684),#206,.T.);
#7847=ADVANCED_FACE('',(#685),#7536,.T.);
#7848=ADVANCED_FACE('',(#686),#70,.F.);
#7849=ADVANCED_FACE('',(#687),#71,.F.);
#7850=ADVANCED_FACE('',(#688),#72,.F.);
#7851=ADVANCED_FACE('',(#689),#7537,.T.);
#7852=ADVANCED_FACE('',(#690),#207,.T.);
#7853=ADVANCED_FACE('',(#691),#373,.F.);
#7854=ADVANCED_FACE('',(#692),#7538,.F.);
#7855=ADVANCED_FACE('',(#693),#374,.F.);
#7856=ADVANCED_FACE('',(#694),#7539,.F.);
#7857=ADVANCED_FACE('',(#695),#375,.F.);
#7858=ADVANCED_FACE('',(#696),#7540,.T.);
#7859=ADVANCED_FACE('',(#697),#220,.T.);
#7860=ADVANCED_FACE('',(#698),#208,.T.);
#7861=ADVANCED_FACE('',(#699),#7541,.T.);
#7862=ADVANCED_FACE('',(#700),#73,.F.);
#7863=ADVANCED_FACE('',(#701),#74,.F.);
#7864=ADVANCED_FACE('',(#702),#75,.F.);
#7865=ADVANCED_FACE('',(#703),#7542,.T.);
#7866=ADVANCED_FACE('',(#704),#209,.T.);
#7867=ADVANCED_FACE('',(#705),#376,.F.);
#7868=ADVANCED_FACE('',(#706),#7543,.F.);
#7869=ADVANCED_FACE('',(#707),#377,.F.);
#7870=ADVANCED_FACE('',(#708),#7544,.F.);
#7871=ADVANCED_FACE('',(#709),#378,.F.);
#7872=ADVANCED_FACE('',(#710),#7545,.T.);
#7873=ADVANCED_FACE('',(#711),#221,.T.);
#7874=ADVANCED_FACE('',(#712),#7546,.T.);
#7875=ADVANCED_FACE('',(#713),#188,.F.);
#7876=ADVANCED_FACE('',(#714),#7547,.T.);
#7877=ADVANCED_FACE('',(#715),#189,.F.);
#7878=ADVANCED_FACE('',(#716),#7548,.T.);
#7879=ADVANCED_FACE('',(#717),#7549,.F.);
#7880=ADVANCED_FACE('',(#718),#379,.F.);
#7881=ADVANCED_FACE('',(#719),#7550,.T.);
#7882=ADVANCED_FACE('',(#720),#190,.F.);
#7883=ADVANCED_FACE('',(#721),#7551,.T.);
#7884=ADVANCED_FACE('',(#722),#191,.F.);
#7885=ADVANCED_FACE('',(#723),#7552,.T.);
#7886=ADVANCED_FACE('',(#724),#380,.F.);
#7887=ADVANCED_FACE('',(#725),#7553,.T.);
#7888=ADVANCED_FACE('',(#726),#222,.T.);
#7889=ADVANCED_FACE('',(#727),#7554,.T.);
#7890=ADVANCED_FACE('',(#728),#192,.F.);
#7891=ADVANCED_FACE('',(#729,#159),#381,.T.);
#7892=ADVANCED_FACE('',(#730),#223,.T.);
#7893=ADVANCED_FACE('',(#731),#7555,.T.);
#7894=ADVANCED_FACE('',(#732),#193,.F.);
#7895=ADVANCED_FACE('',(#733),#7556,.T.);
#7896=ADVANCED_FACE('',(#734),#224,.T.);
#7897=ADVANCED_FACE('',(#735),#7557,.T.);
#7898=ADVANCED_FACE('',(#736),#194,.F.);
#7899=ADVANCED_FACE('',(#737,#160),#382,.T.);
#7900=ADVANCED_FACE('',(#738),#225,.T.);
#7901=ADVANCED_FACE('',(#739),#7558,.T.);
#7902=ADVANCED_FACE('',(#740),#195,.F.);
#7903=ADVANCED_FACE('',(#741),#7559,.T.);
#7904=ADVANCED_FACE('',(#742),#7560,.T.);
#7905=ADVANCED_FACE('',(#743),#383,.T.);
#7906=ADVANCED_FACE('',(#744),#384,.T.);
#7907=ADVANCED_FACE('',(#745),#7561,.T.);
#7908=ADVANCED_FACE('',(#746),#385,.T.);
#7909=ADVANCED_FACE('',(#747),#386,.T.);
#7910=ADVANCED_FACE('',(#748),#387,.T.);
#7911=ADVANCED_FACE('',(#749),#388,.F.);
#7912=ADVANCED_FACE('',(#750),#7562,.T.);
#7913=ADVANCED_FACE('',(#751),#7563,.T.);
#7914=ADVANCED_FACE('',(#752),#7564,.T.);
#7915=ADVANCED_FACE('',(#753),#7565,.T.);
#7916=ADVANCED_FACE('',(#754),#7566,.T.);
#7917=ADVANCED_FACE('',(#755),#7567,.T.);
#7918=ADVANCED_FACE('',(#756),#389,.T.);
#7919=ADVANCED_FACE('',(#757),#7568,.T.);
#7920=ADVANCED_FACE('',(#758),#390,.T.);
#7921=ADVANCED_FACE('',(#759,#161),#391,.F.);
#7922=ADVANCED_FACE('',(#760),#59,.F.);
#7923=ADVANCED_FACE('',(#761),#7569,.F.);
#7924=ADVANCED_FACE('',(#762,#162),#392,.T.);
#7925=ADVANCED_FACE('',(#763),#60,.F.);
#7926=ADVANCED_FACE('',(#764,#163),#393,.F.);
#7927=ADVANCED_FACE('',(#765),#7570,.T.);
#7928=ADVANCED_FACE('',(#766),#76,.F.);
#7929=ADVANCED_FACE('',(#767),#77,.F.);
#7930=ADVANCED_FACE('',(#768),#7571,.T.);
#7931=ADVANCED_FACE('',(#769),#78,.F.);
#7932=ADVANCED_FACE('',(#770),#7572,.T.);
#7933=ADVANCED_FACE('',(#771),#79,.F.);
#7934=ADVANCED_FACE('',(#772),#7573,.T.);
#7935=ADVANCED_FACE('',(#773),#7574,.F.);
#7936=ADVANCED_FACE('',(#774),#226,.T.);
#7937=ADVANCED_FACE('',(#775),#394,.T.);
#7938=ADVANCED_FACE('',(#776),#227,.T.);
#7939=ADVANCED_FACE('',(#777,#164),#395,.F.);
#7940=ADVANCED_FACE('',(#778),#396,.T.);
#7941=ADVANCED_FACE('',(#779),#80,.F.);
#7942=ADVANCED_FACE('',(#780),#81,.F.);
#7943=ADVANCED_FACE('',(#781),#7575,.T.);
#7944=ADVANCED_FACE('',(#782),#82,.F.);
#7945=ADVANCED_FACE('',(#783),#7576,.T.);
#7946=ADVANCED_FACE('',(#784),#83,.F.);
#7947=ADVANCED_FACE('',(#785),#7577,.T.);
#7948=ADVANCED_FACE('',(#786),#228,.T.);
#7949=ADVANCED_FACE('',(#787),#7578,.F.);
#7950=ADVANCED_FACE('',(#788),#7579,.T.);
#7951=ADVANCED_FACE('',(#789,#165),#397,.F.);
#7952=ADVANCED_FACE('',(#790),#398,.T.);
#7953=ADVANCED_FACE('',(#791),#229,.T.);
#7954=ADVANCED_FACE('',(#792),#230,.T.);
#7955=ADVANCED_FACE('',(#793,#166),#399,.F.);
#7956=ADVANCED_FACE('',(#794),#231,.F.);
#7957=ADVANCED_FACE('',(#795),#7580,.T.);
#7958=ADVANCED_FACE('',(#796),#232,.T.);
#7959=ADVANCED_FACE('',(#797,#167),#400,.F.);
#7960=ADVANCED_FACE('',(#798),#61,.F.);
#7961=ADVANCED_FACE('',(#799),#7581,.F.);
#7962=ADVANCED_FACE('',(#800),#7582,.F.);
#7963=ADVANCED_FACE('',(#801),#401,.F.);
#7964=ADVANCED_FACE('',(#802),#7583,.T.);
#7965=ADVANCED_FACE('',(#803),#7584,.T.);
#7966=ADVANCED_FACE('',(#804),#7585,.T.);
#7967=ADVANCED_FACE('',(#805),#7586,.T.);
#7968=ADVANCED_FACE('',(#806),#7587,.T.);
#7969=ADVANCED_FACE('',(#807),#7588,.T.);
#7970=ADVANCED_FACE('',(#808),#7589,.T.);
#7971=ADVANCED_FACE('',(#809),#7590,.T.);
#7972=ADVANCED_FACE('',(#810),#7591,.T.);
#7973=ADVANCED_FACE('',(#811),#7592,.T.);
#7974=ADVANCED_FACE('',(#812),#7593,.T.);
#7975=ADVANCED_FACE('',(#813),#84,.F.);
#7976=ADVANCED_FACE('',(#814),#7594,.T.);
#7977=ADVANCED_FACE('',(#815),#85,.F.);
#7978=ADVANCED_FACE('',(#816,#168),#402,.T.);
#7979=ADVANCED_FACE('',(#817),#7595,.T.);
#7980=ADVANCED_FACE('',(#818,#169),#403,.F.);
#7981=ADVANCED_FACE('',(#819,#170),#404,.T.);
#7982=ADVANCED_FACE('',(#820),#7596,.F.);
#7983=ADVANCED_FACE('',(#821),#7597,.T.);
#7984=ADVANCED_FACE('',(#822),#86,.F.);
#7985=ADVANCED_FACE('',(#823),#87,.F.);
#7986=ADVANCED_FACE('',(#824),#88,.F.);
#7987=ADVANCED_FACE('',(#825),#89,.F.);
#7988=ADVANCED_FACE('',(#826),#7598,.T.);
#7989=ADVANCED_FACE('',(#827),#7599,.T.);
#7990=ADVANCED_FACE('',(#828),#7600,.T.);
#7991=ADVANCED_FACE('',(#829),#7601,.T.);
#7992=ADVANCED_FACE('',(#830),#405,.T.);
#7993=ADVANCED_FACE('',(#831),#7602,.T.);
#7994=ADVANCED_FACE('',(#832),#406,.T.);
#7995=ADVANCED_FACE('',(#833),#7603,.T.);
#7996=ADVANCED_FACE('',(#834,#171),#407,.T.);
#7997=ADVANCED_FACE('',(#835),#408,.T.);
#7998=ADVANCED_FACE('',(#836),#7604,.T.);
#7999=ADVANCED_FACE('',(#837),#409,.T.);
#8000=ADVANCED_FACE('',(#838),#7605,.T.);
#8001=ADVANCED_FACE('',(#839),#7606,.T.);
#8002=ADVANCED_FACE('',(#840),#410,.T.);
#8003=ADVANCED_FACE('',(#841),#7607,.T.);
#8004=ADVANCED_FACE('',(#842),#411,.T.);
#8005=ADVANCED_FACE('',(#843,#172),#412,.F.);
#8006=ADVANCED_FACE('',(#844,#173),#413,.T.);
#8007=ADVANCED_FACE('',(#845),#7608,.F.);
#8008=ADVANCED_FACE('',(#846),#7609,.F.);
#8009=ADVANCED_FACE('',(#847),#7610,.F.);
#8010=ADVANCED_FACE('',(#848),#7611,.F.);
#8011=ADVANCED_FACE('',(#849),#414,.T.);
#8012=ADVANCED_FACE('',(#850),#7612,.T.);
#8013=ADVANCED_FACE('',(#851),#415,.T.);
#8014=ADVANCED_FACE('',(#852),#7613,.T.);
#8015=ADVANCED_FACE('',(#853),#7614,.T.);
#8016=ADVANCED_FACE('',(#854),#416,.F.);
#8017=ADVANCED_FACE('',(#855),#417,.F.);
#8018=ADVANCED_FACE('',(#856),#418,.F.);
#8019=ADVANCED_FACE('',(#857),#7615,.T.);
#8020=ADVANCED_FACE('',(#858),#419,.F.);
#8021=ADVANCED_FACE('',(#859),#420,.F.);
#8022=ADVANCED_FACE('',(#860),#421,.F.);
#8023=ADVANCED_FACE('',(#861),#7616,.T.);
#8024=ADVANCED_FACE('',(#862),#422,.F.);
#8025=ADVANCED_FACE('',(#863),#7617,.T.);
#8026=ADVANCED_FACE('',(#864),#423,.F.);
#8027=ADVANCED_FACE('',(#865),#424,.F.);
#8028=ADVANCED_FACE('',(#866),#425,.F.);
#8029=ADVANCED_FACE('',(#867),#426,.F.);
#8030=ADVANCED_FACE('',(#868),#427,.F.);
#8031=ADVANCED_FACE('',(#869),#428,.F.);
#8032=ADVANCED_FACE('',(#870),#233,.F.);
#8033=ADVANCED_FACE('',(#871,#174),#429,.T.);
#8034=ADVANCED_FACE('',(#872),#7618,.T.);
#8035=ADVANCED_FACE('',(#873),#62,.T.);
#8036=ADVANCED_FACE('',(#874),#7619,.T.);
#8037=ADVANCED_FACE('',(#875),#430,.T.);
#8038=ADVANCED_FACE('',(#876),#210,.T.);
#8039=ADVANCED_FACE('',(#877),#63,.T.);
#8040=ADVANCED_FACE('',(#878),#7620,.T.);
#8041=ADVANCED_FACE('',(#879),#431,.F.);
#8042=ADVANCED_FACE('',(#880),#432,.F.);
#8043=ADVANCED_FACE('',(#881),#433,.F.);
#8044=ADVANCED_FACE('',(#882),#7621,.T.);
#8045=ADVANCED_FACE('',(#883),#434,.F.);
#8046=ADVANCED_FACE('',(#884),#435,.F.);
#8047=ADVANCED_FACE('',(#885),#436,.F.);
#8048=ADVANCED_FACE('',(#886),#7622,.T.);
#8049=ADVANCED_FACE('',(#887),#437,.F.);
#8050=ADVANCED_FACE('',(#888),#7623,.T.);
#8051=ADVANCED_FACE('',(#889),#438,.F.);
#8052=ADVANCED_FACE('',(#890),#439,.F.);
#8053=ADVANCED_FACE('',(#891),#440,.F.);
#8054=ADVANCED_FACE('',(#892),#441,.F.);
#8055=ADVANCED_FACE('',(#893),#442,.F.);
#8056=ADVANCED_FACE('',(#894),#443,.F.);
#8057=ADVANCED_FACE('',(#895),#234,.F.);
#8058=ADVANCED_FACE('',(#896,#175),#444,.T.);
#8059=ADVANCED_FACE('',(#897),#7624,.T.);
#8060=ADVANCED_FACE('',(#898),#64,.T.);
#8061=ADVANCED_FACE('',(#899),#7625,.T.);
#8062=ADVANCED_FACE('',(#900),#445,.T.);
#8063=ADVANCED_FACE('',(#901),#211,.T.);
#8064=ADVANCED_FACE('',(#902),#65,.T.);
#8065=ADVANCED_FACE('',(#903),#7626,.T.);
#8066=ADVANCED_FACE('',(#904),#446,.F.);
#8067=ADVANCED_FACE('',(#905),#447,.F.);
#8068=ADVANCED_FACE('',(#906),#448,.F.);
#8069=ADVANCED_FACE('',(#907),#7627,.T.);
#8070=ADVANCED_FACE('',(#908),#449,.F.);
#8071=ADVANCED_FACE('',(#909),#450,.F.);
#8072=ADVANCED_FACE('',(#910),#451,.F.);
#8073=ADVANCED_FACE('',(#911),#7628,.T.);
#8074=ADVANCED_FACE('',(#912),#452,.F.);
#8075=ADVANCED_FACE('',(#913),#7629,.T.);
#8076=ADVANCED_FACE('',(#914),#453,.F.);
#8077=ADVANCED_FACE('',(#915),#454,.F.);
#8078=ADVANCED_FACE('',(#916),#455,.F.);
#8079=ADVANCED_FACE('',(#917),#456,.F.);
#8080=ADVANCED_FACE('',(#918),#457,.F.);
#8081=ADVANCED_FACE('',(#919),#458,.F.);
#8082=ADVANCED_FACE('',(#920),#235,.F.);
#8083=ADVANCED_FACE('',(#921,#176),#459,.T.);
#8084=ADVANCED_FACE('',(#922),#7630,.T.);
#8085=ADVANCED_FACE('',(#923),#66,.T.);
#8086=ADVANCED_FACE('',(#924),#7631,.T.);
#8087=ADVANCED_FACE('',(#925),#460,.T.);
#8088=ADVANCED_FACE('',(#926),#212,.T.);
#8089=ADVANCED_FACE('',(#927),#67,.T.);
#8090=ADVANCED_FACE('',(#928),#7632,.T.);
#8091=ADVANCED_FACE('',(#929),#461,.F.);
#8092=ADVANCED_FACE('',(#930),#462,.F.);
#8093=ADVANCED_FACE('',(#931),#463,.F.);
#8094=ADVANCED_FACE('',(#932),#7633,.T.);
#8095=ADVANCED_FACE('',(#933),#464,.F.);
#8096=ADVANCED_FACE('',(#934),#465,.F.);
#8097=ADVANCED_FACE('',(#935),#466,.F.);
#8098=ADVANCED_FACE('',(#936),#7634,.T.);
#8099=ADVANCED_FACE('',(#937),#467,.F.);
#8100=ADVANCED_FACE('',(#938),#7635,.T.);
#8101=ADVANCED_FACE('',(#939),#468,.F.);
#8102=ADVANCED_FACE('',(#940),#469,.F.);
#8103=ADVANCED_FACE('',(#941),#470,.F.);
#8104=ADVANCED_FACE('',(#942),#471,.F.);
#8105=ADVANCED_FACE('',(#943),#472,.F.);
#8106=ADVANCED_FACE('',(#944),#473,.F.);
#8107=ADVANCED_FACE('',(#945),#236,.F.);
#8108=ADVANCED_FACE('',(#946,#177),#474,.T.);
#8109=ADVANCED_FACE('',(#947),#7636,.T.);
#8110=ADVANCED_FACE('',(#948),#68,.T.);
#8111=ADVANCED_FACE('',(#949),#7637,.T.);
#8112=ADVANCED_FACE('',(#950),#475,.T.);
#8113=ADVANCED_FACE('',(#951),#213,.T.);
#8114=ADVANCED_FACE('',(#952),#69,.T.);
#8115=CLOSED_SHELL('',(#7638,#7639,#7640,#7641,#7642,#7643,#7644,#7645,
#7646,#7647,#7648,#7649,#7650,#7651,#7652,#7653,#7654,#7655,#7656,#7657,
#7658,#7659,#7660,#7661,#7662,#7663,#7664,#7665,#7666,#7667,#7668,#7669,
#7670,#7671,#7672,#7673,#7674,#7675,#7676,#7677,#7678,#7679,#7680,#7681,
#7682,#7683,#7684,#7685,#7686,#7687,#7688,#7689,#7690,#7691,#7692,#7693,
#7694,#7695,#7696,#7697,#7698,#7699,#7700,#7701,#7702,#7703,#7704,#7705,
#7706,#7707,#7708,#7709,#7710,#7711,#7712,#7713,#7714,#7715,#7716,#7717,
#7718,#7719,#7720,#7721,#7722,#7723,#7724,#7725,#7726,#7727,#7728,#7729,
#7730,#7731,#7732,#7733,#7734,#7735,#7736,#7737,#7738));
#8116=CLOSED_SHELL('',(#7739,#7740,#7741,#7742,#7743,#7744,#7745,#7746,
#7747,#7748,#7749,#7750,#7751,#7752,#7753,#7754,#7755,#7756,#7757,#7758,
#7759,#7760,#7761,#7762,#7763,#7764,#7765,#7766,#7767,#7768,#7769,#7770,
#7771,#7772,#7773,#7774,#7775,#7776,#7777,#7778,#7779,#7780,#7781,#7782,
#7783,#7784,#7785,#7786,#7787,#7788,#7789,#7790,#7791,#7792,#7793,#7794,
#7795,#7796,#7797,#7798,#7799,#7800,#7801,#7802,#7803,#7804,#7805,#7806,
#7807,#7808,#7809,#7810));
#8117=CLOSED_SHELL('',(#7811,#7812,#7813,#7814,#7815,#7816,#7817,#7818,
#7819,#7820,#7821,#7822,#7823,#7824,#7825,#7826,#7827,#7828,#7829,#7830,
#7831,#7832));
#8118=CLOSED_SHELL('',(#7833,#7834,#7835,#7836,#7837,#7838,#7839,#7840,
#7841,#7842,#7843,#7844,#7845,#7846,#7847,#7848,#7849,#7850,#7851,#7852,
#7853,#7854,#7855,#7856,#7857,#7858,#7859,#7860,#7861,#7862,#7863,#7864,
#7865,#7866,#7867,#7868,#7869,#7870,#7871,#7872,#7873,#7874,#7875,#7876,
#7877,#7878,#7879,#7880,#7881,#7882,#7883,#7884,#7885,#7886,#7887,#7888,
#7889,#7890,#7891,#7892,#7893,#7894,#7895,#7896,#7897,#7898,#7899,#7900,
#7901,#7902,#7903,#7904,#7905,#7906,#7907,#7908,#7909,#7910,#7911,#7912,
#7913,#7914,#7915,#7916,#7917,#7918,#7919,#7920,#7921));
#8119=CLOSED_SHELL('',(#7922,#7923,#7924,#7925,#7926,#7927));
#8120=CLOSED_SHELL('',(#7928,#7929,#7930,#7931,#7932,#7933,#7934,#7935,
#7936,#7937,#7938,#7939,#7940,#7941,#7942,#7943,#7944,#7945,#7946,#7947,
#7948,#7949,#7950,#7951,#7952,#7953,#7954,#7955,#7956,#7957,#7958,#7959,
#7960,#7961,#7962,#7963));
#8121=CLOSED_SHELL('',(#7964,#7965,#7966,#7967,#7968,#7969,#7970,#7971,
#7972,#7973,#7974,#7975,#7976,#7977,#7978,#7979,#7980,#7981,#7982,#7983));
#8122=CLOSED_SHELL('',(#7984,#7985,#7986,#7987,#7988,#7989,#7990,#7991,
#7992,#7993,#7994,#7995,#7996,#7997,#7998,#7999,#8000,#8001,#8002,#8003,
#8004,#8005,#8006,#8007,#8008,#8009,#8010,#8011,#8012,#8013,#8014));
#8123=CLOSED_SHELL('',(#8015,#8016,#8017,#8018,#8019,#8020,#8021,#8022,
#8023,#8024,#8025,#8026,#8027,#8028,#8029,#8030,#8031,#8032,#8033,#8034,
#8035,#8036,#8037,#8038,#8039));
#8124=CLOSED_SHELL('',(#8040,#8041,#8042,#8043,#8044,#8045,#8046,#8047,
#8048,#8049,#8050,#8051,#8052,#8053,#8054,#8055,#8056,#8057,#8058,#8059,
#8060,#8061,#8062,#8063,#8064));
#8125=CLOSED_SHELL('',(#8065,#8066,#8067,#8068,#8069,#8070,#8071,#8072,
#8073,#8074,#8075,#8076,#8077,#8078,#8079,#8080,#8081,#8082,#8083,#8084,
#8085,#8086,#8087,#8088,#8089));
#8126=CLOSED_SHELL('',(#8090,#8091,#8092,#8093,#8094,#8095,#8096,#8097,
#8098,#8099,#8100,#8101,#8102,#8103,#8104,#8105,#8106,#8107,#8108,#8109,
#8110,#8111,#8112,#8113,#8114));
#8127=DERIVED_UNIT_ELEMENT(#8151,1.);
#8128=DERIVED_UNIT_ELEMENT(#17044,-3.);
#8129=DERIVED_UNIT_ELEMENT(#8151,1.);
#8130=DERIVED_UNIT_ELEMENT(#17044,-3.);
#8131=DERIVED_UNIT_ELEMENT(#8151,1.);
#8132=DERIVED_UNIT_ELEMENT(#17044,-3.);
#8133=DERIVED_UNIT_ELEMENT(#8151,1.);
#8134=DERIVED_UNIT_ELEMENT(#17044,-3.);
#8135=DERIVED_UNIT_ELEMENT(#8151,1.);
#8136=DERIVED_UNIT_ELEMENT(#17044,-3.);
#8137=DERIVED_UNIT_ELEMENT(#8151,1.);
#8138=DERIVED_UNIT_ELEMENT(#17044,-3.);
#8139=DERIVED_UNIT_ELEMENT(#8151,1.);
#8140=DERIVED_UNIT_ELEMENT(#17044,-3.);
#8141=DERIVED_UNIT_ELEMENT(#8151,1.);
#8142=DERIVED_UNIT_ELEMENT(#17044,-3.);
#8143=DERIVED_UNIT_ELEMENT(#8151,1.);
#8144=DERIVED_UNIT_ELEMENT(#17044,-3.);
#8145=DERIVED_UNIT_ELEMENT(#8151,1.);
#8146=DERIVED_UNIT_ELEMENT(#17044,-3.);
#8147=DERIVED_UNIT_ELEMENT(#8151,1.);
#8148=DERIVED_UNIT_ELEMENT(#17044,-3.);
#8149=DERIVED_UNIT_ELEMENT(#8151,1.);
#8150=DERIVED_UNIT_ELEMENT(#17044,-3.);
#8151=(
MASS_UNIT()
NAMED_UNIT(*)
SI_UNIT(.KILO.,.GRAM.)
);
#8152=DERIVED_UNIT((#8127,#8128));
#8153=DERIVED_UNIT((#8129,#8130));
#8154=DERIVED_UNIT((#8131,#8132));
#8155=DERIVED_UNIT((#8133,#8134));
#8156=DERIVED_UNIT((#8135,#8136));
#8157=DERIVED_UNIT((#8137,#8138));
#8158=DERIVED_UNIT((#8139,#8140));
#8159=DERIVED_UNIT((#8141,#8142));
#8160=DERIVED_UNIT((#8143,#8144));
#8161=DERIVED_UNIT((#8145,#8146));
#8162=DERIVED_UNIT((#8147,#8148));
#8163=DERIVED_UNIT((#8149,#8150));
#8164=MEASURE_REPRESENTATION_ITEM('density measure',
POSITIVE_RATIO_MEASURE(7850.),#8152);
#8165=MEASURE_REPRESENTATION_ITEM('density measure',
POSITIVE_RATIO_MEASURE(7850.),#8153);
#8166=MEASURE_REPRESENTATION_ITEM('density measure',
POSITIVE_RATIO_MEASURE(7850.),#8154);
#8167=MEASURE_REPRESENTATION_ITEM('density measure',
POSITIVE_RATIO_MEASURE(7850.),#8155);
#8168=MEASURE_REPRESENTATION_ITEM('density measure',
POSITIVE_RATIO_MEASURE(7850.),#8156);
#8169=MEASURE_REPRESENTATION_ITEM('density measure',
POSITIVE_RATIO_MEASURE(7850.),#8157);
#8170=MEASURE_REPRESENTATION_ITEM('density measure',
POSITIVE_RATIO_MEASURE(7850.),#8158);
#8171=MEASURE_REPRESENTATION_ITEM('density measure',
POSITIVE_RATIO_MEASURE(7850.),#8159);
#8172=MEASURE_REPRESENTATION_ITEM('density measure',
POSITIVE_RATIO_MEASURE(7750.),#8160);
#8173=MEASURE_REPRESENTATION_ITEM('density measure',
POSITIVE_RATIO_MEASURE(7750.),#8161);
#8174=MEASURE_REPRESENTATION_ITEM('density measure',
POSITIVE_RATIO_MEASURE(7750.),#8162);
#8175=MEASURE_REPRESENTATION_ITEM('density measure',
POSITIVE_RATIO_MEASURE(7750.),#8163);
#8176=PROPERTY_DEFINITION_REPRESENTATION(#8236,#8200);
#8177=PROPERTY_DEFINITION_REPRESENTATION(#8237,#8201);
#8178=PROPERTY_DEFINITION_REPRESENTATION(#8238,#8202);
#8179=PROPERTY_DEFINITION_REPRESENTATION(#8239,#8203);
#8180=PROPERTY_DEFINITION_REPRESENTATION(#8240,#8204);
#8181=PROPERTY_DEFINITION_REPRESENTATION(#8241,#8205);
#8182=PROPERTY_DEFINITION_REPRESENTATION(#8242,#8206);
#8183=PROPERTY_DEFINITION_REPRESENTATION(#8243,#8207);
#8184=PROPERTY_DEFINITION_REPRESENTATION(#8244,#8208);
#8185=PROPERTY_DEFINITION_REPRESENTATION(#8245,#8209);
#8186=PROPERTY_DEFINITION_REPRESENTATION(#8246,#8210);
#8187=PROPERTY_DEFINITION_REPRESENTATION(#8247,#8211);
#8188=PROPERTY_DEFINITION_REPRESENTATION(#8248,#8212);
#8189=PROPERTY_DEFINITION_REPRESENTATION(#8249,#8213);
#8190=PROPERTY_DEFINITION_REPRESENTATION(#8250,#8214);
#8191=PROPERTY_DEFINITION_REPRESENTATION(#8251,#8215);
#8192=PROPERTY_DEFINITION_REPRESENTATION(#8252,#8216);
#8193=PROPERTY_DEFINITION_REPRESENTATION(#8253,#8217);
#8194=PROPERTY_DEFINITION_REPRESENTATION(#8254,#8218);
#8195=PROPERTY_DEFINITION_REPRESENTATION(#8255,#8219);
#8196=PROPERTY_DEFINITION_REPRESENTATION(#8256,#8220);
#8197=PROPERTY_DEFINITION_REPRESENTATION(#8257,#8221);
#8198=PROPERTY_DEFINITION_REPRESENTATION(#8258,#8222);
#8199=PROPERTY_DEFINITION_REPRESENTATION(#8259,#8223);
#8200=REPRESENTATION('material name',(#8224),#17030);
#8201=REPRESENTATION('density',(#8164),#17030);
#8202=REPRESENTATION('material name',(#8225),#17031);
#8203=REPRESENTATION('density',(#8165),#17031);
#8204=REPRESENTATION('material name',(#8226),#17032);
#8205=REPRESENTATION('density',(#8166),#17032);
#8206=REPRESENTATION('material name',(#8227),#17033);
#8207=REPRESENTATION('density',(#8167),#17033);
#8208=REPRESENTATION('material name',(#8228),#17034);
#8209=REPRESENTATION('density',(#8168),#17034);
#8210=REPRESENTATION('material name',(#8229),#17035);
#8211=REPRESENTATION('density',(#8169),#17035);
#8212=REPRESENTATION('material name',(#8230),#17036);
#8213=REPRESENTATION('density',(#8170),#17036);
#8214=REPRESENTATION('material name',(#8231),#17037);
#8215=REPRESENTATION('density',(#8171),#17037);
#8216=REPRESENTATION('material name',(#8232),#17038);
#8217=REPRESENTATION('density',(#8172),#17038);
#8218=REPRESENTATION('material name',(#8233),#17039);
#8219=REPRESENTATION('density',(#8173),#17039);
#8220=REPRESENTATION('material name',(#8234),#17040);
#8221=REPRESENTATION('density',(#8174),#17040);
#8222=REPRESENTATION('material name',(#8235),#17041);
#8223=REPRESENTATION('density',(#8175),#17041);
#8224=DESCRIPTIVE_REPRESENTATION_ITEM('Steel','Steel');
#8225=DESCRIPTIVE_REPRESENTATION_ITEM('Steel','Steel');
#8226=DESCRIPTIVE_REPRESENTATION_ITEM('Steel','Steel');
#8227=DESCRIPTIVE_REPRESENTATION_ITEM('Steel','Steel');
#8228=DESCRIPTIVE_REPRESENTATION_ITEM('Steel','Steel');
#8229=DESCRIPTIVE_REPRESENTATION_ITEM('Steel','Steel');
#8230=DESCRIPTIVE_REPRESENTATION_ITEM('Steel','Steel');
#8231=DESCRIPTIVE_REPRESENTATION_ITEM('Steel','Steel');
#8232=DESCRIPTIVE_REPRESENTATION_ITEM('Steel 4.6, Plain',
'Steel 4.6, Plain');
#8233=DESCRIPTIVE_REPRESENTATION_ITEM('Steel 4.6, Plain',
'Steel 4.6, Plain');
#8234=DESCRIPTIVE_REPRESENTATION_ITEM('Steel 4.6, Plain',
'Steel 4.6, Plain');
#8235=DESCRIPTIVE_REPRESENTATION_ITEM('Steel 4.6, Plain',
'Steel 4.6, Plain');
#8236=PROPERTY_DEFINITION('material property','material name',#17100);
#8237=PROPERTY_DEFINITION('material property','density of part',#17100);
#8238=PROPERTY_DEFINITION('material property','material name',#17101);
#8239=PROPERTY_DEFINITION('material property','density of part',#17101);
#8240=PROPERTY_DEFINITION('material property','material name',#17102);
#8241=PROPERTY_DEFINITION('material property','density of part',#17102);
#8242=PROPERTY_DEFINITION('material property','material name',#17103);
#8243=PROPERTY_DEFINITION('material property','density of part',#17103);
#8244=PROPERTY_DEFINITION('material property','material name',#17104);
#8245=PROPERTY_DEFINITION('material property','density of part',#17104);
#8246=PROPERTY_DEFINITION('material property','material name',#17105);
#8247=PROPERTY_DEFINITION('material property','density of part',#17105);
#8248=PROPERTY_DEFINITION('material property','material name',#17106);
#8249=PROPERTY_DEFINITION('material property','density of part',#17106);
#8250=PROPERTY_DEFINITION('material property','material name',#17107);
#8251=PROPERTY_DEFINITION('material property','density of part',#17107);
#8252=PROPERTY_DEFINITION('material property','material name',#17108);
#8253=PROPERTY_DEFINITION('material property','density of part',#17108);
#8254=PROPERTY_DEFINITION('material property','material name',#17109);
#8255=PROPERTY_DEFINITION('material property','density of part',#17109);
#8256=PROPERTY_DEFINITION('material property','material name',#17110);
#8257=PROPERTY_DEFINITION('material property','density of part',#17110);
#8258=PROPERTY_DEFINITION('material property','material name',#17111);
#8259=PROPERTY_DEFINITION('material property','density of part',#17111);
#8260=AXIS2_PLACEMENT_3D('',#11811,#9251,#9252);
#8261=AXIS2_PLACEMENT_3D('',#11812,#9253,#9254);
#8262=AXIS2_PLACEMENT_3D('',#11813,#9255,#9256);
#8263=AXIS2_PLACEMENT_3D('',#11831,#9258,#9259);
#8264=AXIS2_PLACEMENT_3D('',#11835,#9261,#9262);
#8265=AXIS2_PLACEMENT_3D('',#11838,#9264,#9265);
#8266=AXIS2_PLACEMENT_3D('',#11839,#9266,#9267);
#8267=AXIS2_PLACEMENT_3D('',#11845,#9271,#9272);
#8268=AXIS2_PLACEMENT_3D('',#11855,#9278,#9279);
#8269=AXIS2_PLACEMENT_3D('',#11857,#9280,#9281);
#8270=AXIS2_PLACEMENT_3D('',#11859,#9283,#9284);
#8271=AXIS2_PLACEMENT_3D('',#11865,#9288,#9289);
#8272=AXIS2_PLACEMENT_3D('',#11867,#9290,#9291);
#8273=AXIS2_PLACEMENT_3D('',#11870,#9293,#9294);
#8274=AXIS2_PLACEMENT_3D('',#11871,#9295,#9296);
#8275=AXIS2_PLACEMENT_3D('',#11877,#9300,#9301);
#8276=AXIS2_PLACEMENT_3D('',#11883,#9305,#9306);
#8277=AXIS2_PLACEMENT_3D('',#11893,#9312,#9313);
#8278=AXIS2_PLACEMENT_3D('',#11897,#9315,#9316);
#8279=AXIS2_PLACEMENT_3D('',#11901,#9318,#9319);
#8280=AXIS2_PLACEMENT_3D('',#11911,#9324,#9325);
#8281=AXIS2_PLACEMENT_3D('',#11913,#9326,#9327);
#8282=AXIS2_PLACEMENT_3D('',#11917,#9329,#9330);
#8283=AXIS2_PLACEMENT_3D('',#11918,#9331,#9332);
#8284=AXIS2_PLACEMENT_3D('',#11919,#9333,#9334);
#8285=AXIS2_PLACEMENT_3D('',#11922,#9335,#9336);
#8286=AXIS2_PLACEMENT_3D('',#11926,#9338,#9339);
#8287=AXIS2_PLACEMENT_3D('',#11928,#9341,#9342);
#8288=AXIS2_PLACEMENT_3D('',#11933,#9344,#9345);
#8289=AXIS2_PLACEMENT_3D('',#11936,#9347,#9348);
#8290=AXIS2_PLACEMENT_3D('',#11937,#9349,#9350);
#8291=AXIS2_PLACEMENT_3D('',#11941,#9352,#9353);
#8292=AXIS2_PLACEMENT_3D('',#11943,#9355,#9356);
#8293=AXIS2_PLACEMENT_3D('',#11945,#9357,#9358);
#8294=AXIS2_PLACEMENT_3D('',#11949,#9360,#9361);
#8295=AXIS2_PLACEMENT_3D('',#11951,#9363,#9364);
#8296=AXIS2_PLACEMENT_3D('',#11954,#9365,#9366);
#8297=AXIS2_PLACEMENT_3D('',#11955,#9367,#9368);
#8298=AXIS2_PLACEMENT_3D('',#11956,#9369,#9370);
#8299=AXIS2_PLACEMENT_3D('',#11957,#9371,#9372);
#8300=AXIS2_PLACEMENT_3D('',#11960,#9375,#9376);
#8301=AXIS2_PLACEMENT_3D('',#11963,#9377,#9378);
#8302=AXIS2_PLACEMENT_3D('',#11964,#9379,#9380);
#8303=AXIS2_PLACEMENT_3D('',#11965,#9381,#9382);
#8304=AXIS2_PLACEMENT_3D('',#11966,#9383,#9384);
#8305=AXIS2_PLACEMENT_3D('',#11969,#9385,#9386);
#8306=AXIS2_PLACEMENT_3D('',#11972,#9389,#9390);
#8307=AXIS2_PLACEMENT_3D('',#11973,#9391,#9392);
#8308=AXIS2_PLACEMENT_3D('',#11974,#9393,#9394);
#8309=AXIS2_PLACEMENT_3D('',#11976,#9395,#9396);
#8310=AXIS2_PLACEMENT_3D('',#11980,#9398,#9399);
#8311=AXIS2_PLACEMENT_3D('',#11982,#9401,#9402);
#8312=AXIS2_PLACEMENT_3D('',#11983,#9403,#9404);
#8313=AXIS2_PLACEMENT_3D('',#11984,#9405,#9406);
#8314=AXIS2_PLACEMENT_3D('',#11999,#9415,#9416);
#8315=AXIS2_PLACEMENT_3D('',#12002,#9418,#9419);
#8316=AXIS2_PLACEMENT_3D('',#12003,#9420,#9421);
#8317=AXIS2_PLACEMENT_3D('',#12009,#9424,#9425);
#8318=AXIS2_PLACEMENT_3D('',#12011,#9426,#9427);
#8319=AXIS2_PLACEMENT_3D('',#12015,#9429,#9430);
#8320=AXIS2_PLACEMENT_3D('',#12019,#9432,#9433);
#8321=AXIS2_PLACEMENT_3D('',#12025,#9436,#9437);
#8322=AXIS2_PLACEMENT_3D('',#12027,#9439,#9440);
#8323=AXIS2_PLACEMENT_3D('',#12030,#9442,#9443);
#8324=AXIS2_PLACEMENT_3D('',#12031,#9444,#9445);
#8325=AXIS2_PLACEMENT_3D('',#12043,#9452,#9453);
#8326=AXIS2_PLACEMENT_3D('',#12052,#9458,#9459);
#8327=AXIS2_PLACEMENT_3D('',#12061,#9464,#9465);
#8328=AXIS2_PLACEMENT_3D('',#12062,#9466,#9467);
#8329=AXIS2_PLACEMENT_3D('',#12063,#9468,#9469);
#8330=AXIS2_PLACEMENT_3D('',#12064,#9470,#9471);
#8331=AXIS2_PLACEMENT_3D('',#12070,#9475,#9476);
#8332=AXIS2_PLACEMENT_3D('',#12071,#9477,#9478);
#8333=AXIS2_PLACEMENT_3D('',#12072,#9479,#9480);
#8334=AXIS2_PLACEMENT_3D('',#12073,#9481,#9482);
#8335=AXIS2_PLACEMENT_3D('',#12081,#9487,#9488);
#8336=AXIS2_PLACEMENT_3D('',#12083,#9489,#9490);
#8337=AXIS2_PLACEMENT_3D('',#12087,#9492,#9493);
#8338=AXIS2_PLACEMENT_3D('',#12091,#9495,#9496);
#8339=AXIS2_PLACEMENT_3D('',#12096,#9499,#9500);
#8340=AXIS2_PLACEMENT_3D('',#12100,#9502,#9503);
#8341=AXIS2_PLACEMENT_3D('',#12103,#9505,#9506);
#8342=AXIS2_PLACEMENT_3D('',#12105,#9507,#9508);
#8343=AXIS2_PLACEMENT_3D('',#12107,#9510,#9511);
#8344=AXIS2_PLACEMENT_3D('',#12109,#9512,#9513);
#8345=AXIS2_PLACEMENT_3D('',#12113,#9515,#9516);
#8346=AXIS2_PLACEMENT_3D('',#12117,#9519,#9520);
#8347=AXIS2_PLACEMENT_3D('',#12118,#9521,#9522);
#8348=AXIS2_PLACEMENT_3D('',#12120,#9523,#9524);
#8349=AXIS2_PLACEMENT_3D('',#12124,#9526,#9527);
#8350=AXIS2_PLACEMENT_3D('',#12126,#9529,#9530);
#8351=AXIS2_PLACEMENT_3D('',#12127,#9531,#9532);
#8352=AXIS2_PLACEMENT_3D('',#12129,#9533,#9534);
#8353=AXIS2_PLACEMENT_3D('',#12134,#9537,#9538);
#8354=AXIS2_PLACEMENT_3D('',#12136,#9540,#9541);
#8355=AXIS2_PLACEMENT_3D('',#12138,#9542,#9543);
#8356=AXIS2_PLACEMENT_3D('',#12142,#9546,#9547);
#8357=AXIS2_PLACEMENT_3D('',#12143,#9548,#9549);
#8358=AXIS2_PLACEMENT_3D('',#12147,#9552,#9553);
#8359=AXIS2_PLACEMENT_3D('',#12151,#9556,#9557);
#8360=AXIS2_PLACEMENT_3D('',#12157,#9560,#9561);
#8361=AXIS2_PLACEMENT_3D('',#12161,#9564,#9565);
#8362=AXIS2_PLACEMENT_3D('',#12167,#9569,#9570);
#8363=AXIS2_PLACEMENT_3D('',#12175,#9575,#9576);
#8364=AXIS2_PLACEMENT_3D('',#12179,#9579,#9580);
#8365=AXIS2_PLACEMENT_3D('',#12183,#9583,#9584);
#8366=AXIS2_PLACEMENT_3D('',#12186,#9585,#9586);
#8367=AXIS2_PLACEMENT_3D('',#12195,#9591,#9592);
#8368=AXIS2_PLACEMENT_3D('',#12199,#9595,#9596);
#8369=AXIS2_PLACEMENT_3D('',#12202,#9598,#9599);
#8370=AXIS2_PLACEMENT_3D('',#12203,#9600,#9601);
#8371=AXIS2_PLACEMENT_3D('',#12205,#9603,#9604);
#8372=AXIS2_PLACEMENT_3D('',#12207,#9605,#9606);
#8373=AXIS2_PLACEMENT_3D('',#12209,#9608,#9609);
#8374=AXIS2_PLACEMENT_3D('',#12211,#9610,#9611);
#8375=AXIS2_PLACEMENT_3D('',#12213,#9613,#9614);
#8376=AXIS2_PLACEMENT_3D('',#12215,#9616,#9617);
#8377=AXIS2_PLACEMENT_3D('',#12219,#9620,#9621);
#8378=AXIS2_PLACEMENT_3D('',#12221,#9623,#9624);
#8379=AXIS2_PLACEMENT_3D('',#12223,#9626,#9627);
#8380=AXIS2_PLACEMENT_3D('',#12224,#9628,#9629);
#8381=AXIS2_PLACEMENT_3D('',#12228,#9632,#9633);
#8382=AXIS2_PLACEMENT_3D('',#12232,#9636,#9637);
#8383=AXIS2_PLACEMENT_3D('',#12233,#9638,#9639);
#8384=AXIS2_PLACEMENT_3D('',#12234,#9640,#9641);
#8385=AXIS2_PLACEMENT_3D('',#12235,#9642,#9643);
#8386=AXIS2_PLACEMENT_3D('',#12236,#9644,#9645);
#8387=AXIS2_PLACEMENT_3D('',#12238,#9646,#9647);
#8388=AXIS2_PLACEMENT_3D('',#12241,#9649,#9650);
#8389=AXIS2_PLACEMENT_3D('',#12242,#9651,#9652);
#8390=AXIS2_PLACEMENT_3D('',#12244,#9653,#9654);
#8391=AXIS2_PLACEMENT_3D('',#12245,#9655,#9656);
#8392=AXIS2_PLACEMENT_3D('',#12246,#9657,#9658);
#8393=AXIS2_PLACEMENT_3D('',#12248,#9659,#9660);
#8394=AXIS2_PLACEMENT_3D('',#12250,#9662,#9663);
#8395=AXIS2_PLACEMENT_3D('',#12252,#9664,#9665);
#8396=AXIS2_PLACEMENT_3D('',#12254,#9666,#9667);
#8397=AXIS2_PLACEMENT_3D('',#12255,#9668,#9669);
#8398=AXIS2_PLACEMENT_3D('',#12256,#9670,#9671);
#8399=AXIS2_PLACEMENT_3D('',#12258,#9672,#9673);
#8400=AXIS2_PLACEMENT_3D('',#12269,#9675,#9676);
#8401=AXIS2_PLACEMENT_3D('',#12270,#9677,#9678);
#8402=AXIS2_PLACEMENT_3D('',#12271,#9679,#9680);
#8403=AXIS2_PLACEMENT_3D('',#12272,#9681,#9682);
#8404=AXIS2_PLACEMENT_3D('',#12282,#9683,#9684);
#8405=AXIS2_PLACEMENT_3D('',#12283,#9685,#9686);
#8406=AXIS2_PLACEMENT_3D('',#12284,#9687,#9688);
#8407=AXIS2_PLACEMENT_3D('',#12285,#9689,#9690);
#8408=AXIS2_PLACEMENT_3D('',#12286,#9691,#9692);
#8409=AXIS2_PLACEMENT_3D('',#12288,#9693,#9694);
#8410=AXIS2_PLACEMENT_3D('',#12291,#9696,#9697);
#8411=AXIS2_PLACEMENT_3D('',#12292,#9698,#9699);
#8412=AXIS2_PLACEMENT_3D('',#12294,#9700,#9701);
#8413=AXIS2_PLACEMENT_3D('',#12295,#9702,#9703);
#8414=AXIS2_PLACEMENT_3D('',#12296,#9704,#9705);
#8415=AXIS2_PLACEMENT_3D('',#12297,#9706,#9707);
#8416=AXIS2_PLACEMENT_3D('',#12298,#9708,#9709);
#8417=AXIS2_PLACEMENT_3D('',#12299,#9710,#9711);
#8418=AXIS2_PLACEMENT_3D('',#12300,#9712,#9713);
#8419=AXIS2_PLACEMENT_3D('',#12301,#9714,#9715);
#8420=AXIS2_PLACEMENT_3D('',#12302,#9716,#9717);
#8421=AXIS2_PLACEMENT_3D('',#12303,#9718,#9719);
#8422=AXIS2_PLACEMENT_3D('',#12304,#9720,#9721);
#8423=AXIS2_PLACEMENT_3D('',#12307,#9723,#9724);
#8424=AXIS2_PLACEMENT_3D('',#12308,#9725,#9726);
#8425=AXIS2_PLACEMENT_3D('',#12312,#9729,#9730);
#8426=AXIS2_PLACEMENT_3D('',#12315,#9732,#9733);
#8427=AXIS2_PLACEMENT_3D('',#12316,#9734,#9735);
#8428=AXIS2_PLACEMENT_3D('',#12320,#9738,#9739);
#8429=AXIS2_PLACEMENT_3D('',#12321,#9740,#9741);
#8430=AXIS2_PLACEMENT_3D('',#12322,#9742,#9743);
#8431=AXIS2_PLACEMENT_3D('',#12323,#9744,#9745);
#8432=AXIS2_PLACEMENT_3D('',#12325,#9747,#9748);
#8433=AXIS2_PLACEMENT_3D('',#12327,#9750,#9751);
#8434=AXIS2_PLACEMENT_3D('',#12331,#9753,#9754);
#8435=AXIS2_PLACEMENT_3D('',#12333,#9756,#9757);
#8436=AXIS2_PLACEMENT_3D('',#12336,#9759,#9760);
#8437=AXIS2_PLACEMENT_3D('',#12337,#9761,#9762);
#8438=AXIS2_PLACEMENT_3D('',#12340,#9764,#9765);
#8439=AXIS2_PLACEMENT_3D('',#12341,#9766,#9767);
#8440=AXIS2_PLACEMENT_3D('',#12345,#9770,#9771);
#8441=AXIS2_PLACEMENT_3D('',#12346,#9772,#9773);
#8442=AXIS2_PLACEMENT_3D('',#12347,#9774,#9775);
#8443=AXIS2_PLACEMENT_3D('',#12351,#9778,#9779);
#8444=AXIS2_PLACEMENT_3D('',#12357,#9783,#9784);
#8445=AXIS2_PLACEMENT_3D('',#12358,#9785,#9786);
#8446=AXIS2_PLACEMENT_3D('',#12359,#9787,#9788);
#8447=AXIS2_PLACEMENT_3D('',#12361,#9789,#9790);
#8448=AXIS2_PLACEMENT_3D('',#12363,#9792,#9793);
#8449=AXIS2_PLACEMENT_3D('',#12366,#9795,#9796);
#8450=AXIS2_PLACEMENT_3D('',#12367,#9797,#9798);
#8451=AXIS2_PLACEMENT_3D('',#12371,#9801,#9802);
#8452=AXIS2_PLACEMENT_3D('',#12374,#9804,#9805);
#8453=AXIS2_PLACEMENT_3D('',#12375,#9806,#9807);
#8454=AXIS2_PLACEMENT_3D('',#12379,#9810,#9811);
#8455=AXIS2_PLACEMENT_3D('',#12382,#9813,#9814);
#8456=AXIS2_PLACEMENT_3D('',#12383,#9815,#9816);
#8457=AXIS2_PLACEMENT_3D('',#12384,#9817,#9818);
#8458=AXIS2_PLACEMENT_3D('',#12386,#9820,#9821);
#8459=AXIS2_PLACEMENT_3D('',#12389,#9824,#9825);
#8460=AXIS2_PLACEMENT_3D('',#12390,#9826,#9827);
#8461=AXIS2_PLACEMENT_3D('',#12391,#9828,#9829);
#8462=AXIS2_PLACEMENT_3D('',#12392,#9830,#9831);
#8463=AXIS2_PLACEMENT_3D('',#12393,#9832,#9833);
#8464=AXIS2_PLACEMENT_3D('',#12400,#9836,#9837);
#8465=AXIS2_PLACEMENT_3D('',#12404,#9839,#9840);
#8466=AXIS2_PLACEMENT_3D('',#12408,#9842,#9843);
#8467=AXIS2_PLACEMENT_3D('',#12412,#9845,#9846);
#8468=AXIS2_PLACEMENT_3D('',#12422,#9851,#9852);
#8469=AXIS2_PLACEMENT_3D('',#12424,#9853,#9854);
#8470=AXIS2_PLACEMENT_3D('',#12427,#9856,#9857);
#8471=AXIS2_PLACEMENT_3D('',#12429,#9858,#9859);
#8472=AXIS2_PLACEMENT_3D('',#12431,#9860,#9861);
#8473=AXIS2_PLACEMENT_3D('',#12443,#9862,#9863);
#8474=AXIS2_PLACEMENT_3D('',#12445,#9864,#9865);
#8475=AXIS2_PLACEMENT_3D('',#12447,#9866,#9867);
#8476=AXIS2_PLACEMENT_3D('',#12448,#9868,#9869);
#8477=AXIS2_PLACEMENT_3D('',#12449,#9870,#9871);
#8478=AXIS2_PLACEMENT_3D('',#12452,#9872,#9873);
#8479=AXIS2_PLACEMENT_3D('',#12466,#9876,#9877);
#8480=AXIS2_PLACEMENT_3D('',#12468,#9878,#9879);
#8481=AXIS2_PLACEMENT_3D('',#12470,#9880,#9881);
#8482=AXIS2_PLACEMENT_3D('',#12471,#9882,#9883);
#8483=AXIS2_PLACEMENT_3D('',#12472,#9884,#9885);
#8484=AXIS2_PLACEMENT_3D('',#12477,#9888,#9889);
#8485=AXIS2_PLACEMENT_3D('',#12478,#9890,#9891);
#8486=AXIS2_PLACEMENT_3D('',#12482,#9893,#9894);
#8487=AXIS2_PLACEMENT_3D('',#12493,#9896,#9897);
#8488=AXIS2_PLACEMENT_3D('',#12494,#9898,#9899);
#8489=AXIS2_PLACEMENT_3D('',#12495,#9900,#9901);
#8490=AXIS2_PLACEMENT_3D('',#12499,#9903,#9904);
#8491=AXIS2_PLACEMENT_3D('',#12501,#9906,#9907);
#8492=AXIS2_PLACEMENT_3D('',#12505,#9910,#9911);
#8493=AXIS2_PLACEMENT_3D('',#12510,#9914,#9915);
#8494=AXIS2_PLACEMENT_3D('',#12511,#9916,#9917);
#8495=AXIS2_PLACEMENT_3D('',#12516,#9920,#9921);
#8496=AXIS2_PLACEMENT_3D('',#12517,#9922,#9923);
#8497=AXIS2_PLACEMENT_3D('',#12527,#9929,#9930);
#8498=AXIS2_PLACEMENT_3D('',#12530,#9933,#9934);
#8499=AXIS2_PLACEMENT_3D('',#12533,#9936,#9937);
#8500=AXIS2_PLACEMENT_3D('',#12534,#9938,#9939);
#8501=AXIS2_PLACEMENT_3D('',#12535,#9940,#9941);
#8502=AXIS2_PLACEMENT_3D('',#12546,#9947,#9948);
#8503=AXIS2_PLACEMENT_3D('',#12549,#9950,#9951);
#8504=AXIS2_PLACEMENT_3D('',#12551,#9953,#9954);
#8505=AXIS2_PLACEMENT_3D('',#12553,#9955,#9956);
#8506=AXIS2_PLACEMENT_3D('',#12555,#9958,#9959);
#8507=AXIS2_PLACEMENT_3D('',#12556,#9960,#9961);
#8508=AXIS2_PLACEMENT_3D('',#12560,#9964,#9965);
#8509=AXIS2_PLACEMENT_3D('',#12566,#9969,#9970);
#8510=AXIS2_PLACEMENT_3D('',#12582,#9971,#9972);
#8511=AXIS2_PLACEMENT_3D('',#12583,#9973,#9974);
#8512=AXIS2_PLACEMENT_3D('',#12584,#9975,#9976);
#8513=AXIS2_PLACEMENT_3D('',#12585,#9977,#9978);
#8514=AXIS2_PLACEMENT_3D('',#12589,#9980,#9981);
#8515=AXIS2_PLACEMENT_3D('',#12593,#9983,#9984);
#8516=AXIS2_PLACEMENT_3D('',#12603,#9989,#9990);
#8517=AXIS2_PLACEMENT_3D('',#12606,#9992,#9993);
#8518=AXIS2_PLACEMENT_3D('',#12608,#9994,#9995);
#8519=AXIS2_PLACEMENT_3D('',#12610,#9996,#9997);
#8520=AXIS2_PLACEMENT_3D('',#12611,#9998,#9999);
#8521=AXIS2_PLACEMENT_3D('',#12614,#10000,#10001);
#8522=AXIS2_PLACEMENT_3D('',#12618,#10003,#10004);
#8523=AXIS2_PLACEMENT_3D('',#12620,#10006,#10007);
#8524=AXIS2_PLACEMENT_3D('',#12623,#10010,#10011);
#8525=AXIS2_PLACEMENT_3D('',#12629,#10015,#10016);
#8526=AXIS2_PLACEMENT_3D('',#12631,#10017,#10018);
#8527=AXIS2_PLACEMENT_3D('',#12633,#10019,#10020);
#8528=AXIS2_PLACEMENT_3D('',#12635,#10022,#10023);
#8529=AXIS2_PLACEMENT_3D('',#12638,#10026,#10027);
#8530=AXIS2_PLACEMENT_3D('',#12644,#10031,#10032);
#8531=AXIS2_PLACEMENT_3D('',#12650,#10036,#10037);
#8532=AXIS2_PLACEMENT_3D('',#12652,#10038,#10039);
#8533=AXIS2_PLACEMENT_3D('',#12656,#10041,#10042);
#8534=AXIS2_PLACEMENT_3D('',#12658,#10043,#10044);
#8535=AXIS2_PLACEMENT_3D('',#12666,#10048,#10049);
#8536=AXIS2_PLACEMENT_3D('',#12669,#10051,#10052);
#8537=AXIS2_PLACEMENT_3D('',#12670,#10053,#10054);
#8538=AXIS2_PLACEMENT_3D('',#12673,#10057,#10058);
#8539=AXIS2_PLACEMENT_3D('',#12676,#10061,#10062);
#8540=AXIS2_PLACEMENT_3D('',#12679,#10065,#10066);
#8541=AXIS2_PLACEMENT_3D('',#12682,#10069,#10070);
#8542=AXIS2_PLACEMENT_3D('',#12684,#10072,#10073);
#8543=AXIS2_PLACEMENT_3D('',#12685,#10074,#10075);
#8544=AXIS2_PLACEMENT_3D('',#12686,#10076,#10077);
#8545=AXIS2_PLACEMENT_3D('',#12687,#10078,#10079);
#8546=AXIS2_PLACEMENT_3D('',#12688,#10080,#10081);
#8547=AXIS2_PLACEMENT_3D('',#12689,#10082,#10083);
#8548=AXIS2_PLACEMENT_3D('',#12692,#10085,#10086);
#8549=AXIS2_PLACEMENT_3D('',#12693,#10087,#10088);
#8550=AXIS2_PLACEMENT_3D('',#12694,#10089,#10090);
#8551=AXIS2_PLACEMENT_3D('',#12697,#10092,#10093);
#8552=AXIS2_PLACEMENT_3D('',#12698,#10094,#10095);
#8553=AXIS2_PLACEMENT_3D('',#12699,#10096,#10097);
#8554=AXIS2_PLACEMENT_3D('',#12702,#10099,#10100);
#8555=AXIS2_PLACEMENT_3D('',#12703,#10101,#10102);
#8556=AXIS2_PLACEMENT_3D('',#12704,#10103,#10104);
#8557=AXIS2_PLACEMENT_3D('',#12707,#10106,#10107);
#8558=AXIS2_PLACEMENT_3D('',#12708,#10108,#10109);
#8559=AXIS2_PLACEMENT_3D('',#12709,#10110,#10111);
#8560=AXIS2_PLACEMENT_3D('',#12712,#10112,#10113);
#8561=AXIS2_PLACEMENT_3D('',#12716,#10115,#10116);
#8562=AXIS2_PLACEMENT_3D('',#12718,#10118,#10119);
#8563=AXIS2_PLACEMENT_3D('',#12721,#10120,#10121);
#8564=AXIS2_PLACEMENT_3D('',#12722,#10122,#10123);
#8565=AXIS2_PLACEMENT_3D('',#12723,#10124,#10125);
#8566=AXIS2_PLACEMENT_3D('',#12724,#10126,#10127);
#8567=AXIS2_PLACEMENT_3D('',#12727,#10128,#10129);
#8568=AXIS2_PLACEMENT_3D('',#12741,#10132,#10133);
#8569=AXIS2_PLACEMENT_3D('',#12742,#10134,#10135);
#8570=AXIS2_PLACEMENT_3D('',#12743,#10136,#10137);
#8571=AXIS2_PLACEMENT_3D('',#12744,#10138,#10139);
#8572=AXIS2_PLACEMENT_3D('',#12747,#10140,#10141);
#8573=AXIS2_PLACEMENT_3D('',#12760,#10144,#10145);
#8574=AXIS2_PLACEMENT_3D('',#12761,#10146,#10147);
#8575=AXIS2_PLACEMENT_3D('',#12762,#10148,#10149);
#8576=AXIS2_PLACEMENT_3D('',#12763,#10150,#10151);
#8577=AXIS2_PLACEMENT_3D('',#12765,#10152,#10153);
#8578=AXIS2_PLACEMENT_3D('',#12778,#10155,#10156);
#8579=AXIS2_PLACEMENT_3D('',#12779,#10157,#10158);
#8580=AXIS2_PLACEMENT_3D('',#12780,#10159,#10160);
#8581=AXIS2_PLACEMENT_3D('',#12781,#10161,#10162);
#8582=AXIS2_PLACEMENT_3D('',#12784,#10163,#10164);
#8583=AXIS2_PLACEMENT_3D('',#12797,#10167,#10168);
#8584=AXIS2_PLACEMENT_3D('',#12798,#10169,#10170);
#8585=AXIS2_PLACEMENT_3D('',#12799,#10171,#10172);
#8586=AXIS2_PLACEMENT_3D('',#12800,#10173,#10174);
#8587=AXIS2_PLACEMENT_3D('',#12802,#10175,#10176);
#8588=AXIS2_PLACEMENT_3D('',#12813,#10178,#10179);
#8589=AXIS2_PLACEMENT_3D('',#12814,#10180,#10181);
#8590=AXIS2_PLACEMENT_3D('',#12815,#10182,#10183);
#8591=AXIS2_PLACEMENT_3D('',#12817,#10185,#10186);
#8592=AXIS2_PLACEMENT_3D('',#12819,#10188,#10189);
#8593=AXIS2_PLACEMENT_3D('',#12821,#10191,#10192);
#8594=AXIS2_PLACEMENT_3D('',#12823,#10194,#10195);
#8595=AXIS2_PLACEMENT_3D('',#12825,#10197,#10198);
#8596=AXIS2_PLACEMENT_3D('',#12827,#10200,#10201);
#8597=AXIS2_PLACEMENT_3D('',#12828,#10202,#10203);
#8598=AXIS2_PLACEMENT_3D('',#12829,#10204,#10205);
#8599=AXIS2_PLACEMENT_3D('',#12831,#10207,#10208);
#8600=AXIS2_PLACEMENT_3D('',#12833,#10210,#10211);
#8601=AXIS2_PLACEMENT_3D('',#12834,#10212,#10213);
#8602=AXIS2_PLACEMENT_3D('',#12835,#10214,#10215);
#8603=AXIS2_PLACEMENT_3D('',#12837,#10216,#10217);
#8604=AXIS2_PLACEMENT_3D('',#12840,#10219,#10220);
#8605=AXIS2_PLACEMENT_3D('',#12841,#10221,#10222);
#8606=AXIS2_PLACEMENT_3D('',#12843,#10223,#10224);
#8607=AXIS2_PLACEMENT_3D('',#12846,#10226,#10227);
#8608=AXIS2_PLACEMENT_3D('',#12847,#10228,#10229);
#8609=AXIS2_PLACEMENT_3D('',#12849,#10230,#10231);
#8610=AXIS2_PLACEMENT_3D('',#12852,#10233,#10234);
#8611=AXIS2_PLACEMENT_3D('',#12853,#10235,#10236);
#8612=AXIS2_PLACEMENT_3D('',#12855,#10237,#10238);
#8613=AXIS2_PLACEMENT_3D('',#12858,#10240,#10241);
#8614=AXIS2_PLACEMENT_3D('',#12859,#10242,#10243);
#8615=AXIS2_PLACEMENT_3D('',#12862,#10244,#10245);
#8616=AXIS2_PLACEMENT_3D('',#12866,#10247,#10248);
#8617=AXIS2_PLACEMENT_3D('',#12870,#10250,#10251);
#8618=AXIS2_PLACEMENT_3D('',#12874,#10253,#10254);
#8619=AXIS2_PLACEMENT_3D('',#12878,#10256,#10257);
#8620=AXIS2_PLACEMENT_3D('',#12882,#10259,#10260);
#8621=AXIS2_PLACEMENT_3D('',#12886,#10262,#10263);
#8622=AXIS2_PLACEMENT_3D('',#12890,#10265,#10266);
#8623=AXIS2_PLACEMENT_3D('',#12892,#10268,#10269);
#8624=AXIS2_PLACEMENT_3D('',#12898,#10273,#10274);
#8625=AXIS2_PLACEMENT_3D('',#12900,#10275,#10276);
#8626=AXIS2_PLACEMENT_3D('',#12902,#10278,#10279);
#8627=AXIS2_PLACEMENT_3D('',#12906,#10282,#10283);
#8628=AXIS2_PLACEMENT_3D('',#12908,#10284,#10285);
#8629=AXIS2_PLACEMENT_3D('',#12910,#10287,#10288);
#8630=AXIS2_PLACEMENT_3D('',#12914,#10291,#10292);
#8631=AXIS2_PLACEMENT_3D('',#12916,#10293,#10294);
#8632=AXIS2_PLACEMENT_3D('',#12918,#10296,#10297);
#8633=AXIS2_PLACEMENT_3D('',#12922,#10300,#10301);
#8634=AXIS2_PLACEMENT_3D('',#12923,#10302,#10303);
#8635=AXIS2_PLACEMENT_3D('',#12924,#10304,#10305);
#8636=AXIS2_PLACEMENT_3D('',#12930,#10309,#10310);
#8637=AXIS2_PLACEMENT_3D('',#12932,#10311,#10312);
#8638=AXIS2_PLACEMENT_3D('',#12934,#10314,#10315);
#8639=AXIS2_PLACEMENT_3D('',#12938,#10318,#10319);
#8640=AXIS2_PLACEMENT_3D('',#12940,#10320,#10321);
#8641=AXIS2_PLACEMENT_3D('',#12942,#10323,#10324);
#8642=AXIS2_PLACEMENT_3D('',#12946,#10327,#10328);
#8643=AXIS2_PLACEMENT_3D('',#12948,#10329,#10330);
#8644=AXIS2_PLACEMENT_3D('',#12950,#10332,#10333);
#8645=AXIS2_PLACEMENT_3D('',#12954,#10336,#10337);
#8646=AXIS2_PLACEMENT_3D('',#12955,#10338,#10339);
#8647=AXIS2_PLACEMENT_3D('',#12956,#10340,#10341);
#8648=AXIS2_PLACEMENT_3D('',#12957,#10342,#10343);
#8649=AXIS2_PLACEMENT_3D('',#12958,#10344,#10345);
#8650=AXIS2_PLACEMENT_3D('',#12961,#10346,#10347);
#8651=AXIS2_PLACEMENT_3D('',#12965,#10349,#10350);
#8652=AXIS2_PLACEMENT_3D('',#12967,#10352,#10353);
#8653=AXIS2_PLACEMENT_3D('',#12969,#10354,#10355);
#8654=AXIS2_PLACEMENT_3D('',#12973,#10357,#10358);
#8655=AXIS2_PLACEMENT_3D('',#12975,#10360,#10361);
#8656=AXIS2_PLACEMENT_3D('',#12976,#10362,#10363);
#8657=AXIS2_PLACEMENT_3D('',#12977,#10364,#10365);
#8658=AXIS2_PLACEMENT_3D('',#12979,#10366,#10367);
#8659=AXIS2_PLACEMENT_3D('',#12983,#10369,#10370);
#8660=AXIS2_PLACEMENT_3D('',#12985,#10372,#10373);
#8661=AXIS2_PLACEMENT_3D('',#12986,#10374,#10375);
#8662=AXIS2_PLACEMENT_3D('',#12987,#10376,#10377);
#8663=AXIS2_PLACEMENT_3D('',#12989,#10378,#10379);
#8664=AXIS2_PLACEMENT_3D('',#12992,#10381,#10382);
#8665=AXIS2_PLACEMENT_3D('',#12994,#10384,#10385);
#8666=AXIS2_PLACEMENT_3D('',#12995,#10386,#10387);
#8667=AXIS2_PLACEMENT_3D('',#12996,#10388,#10389);
#8668=AXIS2_PLACEMENT_3D('',#12997,#10390,#10391);
#8669=AXIS2_PLACEMENT_3D('',#12998,#10392,#10393);
#8670=AXIS2_PLACEMENT_3D('',#13002,#10395,#10396);
#8671=AXIS2_PLACEMENT_3D('',#13004,#10398,#10399);
#8672=AXIS2_PLACEMENT_3D('',#13008,#10402,#10403);
#8673=AXIS2_PLACEMENT_3D('',#13011,#10405,#10406);
#8674=AXIS2_PLACEMENT_3D('',#13012,#10407,#10408);
#8675=AXIS2_PLACEMENT_3D('',#13016,#10411,#10412);
#8676=AXIS2_PLACEMENT_3D('',#13018,#10413,#10414);
#8677=AXIS2_PLACEMENT_3D('',#13019,#10415,#10416);
#8678=AXIS2_PLACEMENT_3D('',#13022,#10417,#10418);
#8679=AXIS2_PLACEMENT_3D('',#13024,#10419,#10420);
#8680=AXIS2_PLACEMENT_3D('',#13025,#10421,#10422);
#8681=AXIS2_PLACEMENT_3D('',#13026,#10423,#10424);
#8682=AXIS2_PLACEMENT_3D('',#13029,#10425,#10426);
#8683=AXIS2_PLACEMENT_3D('',#13069,#10429,#10430);
#8684=AXIS2_PLACEMENT_3D('',#13124,#10431,#10432);
#8685=AXIS2_PLACEMENT_3D('',#13125,#10433,#10434);
#8686=AXIS2_PLACEMENT_3D('',#13126,#10435,#10436);
#8687=AXIS2_PLACEMENT_3D('',#13164,#10437,#10438);
#8688=AXIS2_PLACEMENT_3D('',#13175,#10439,#10440);
#8689=AXIS2_PLACEMENT_3D('',#13178,#10441,#10442);
#8690=AXIS2_PLACEMENT_3D('',#13181,#10445,#10446);
#8691=AXIS2_PLACEMENT_3D('',#13183,#10447,#10448);
#8692=AXIS2_PLACEMENT_3D('',#13184,#10449,#10450);
#8693=AXIS2_PLACEMENT_3D('',#13185,#10451,#10452);
#8694=AXIS2_PLACEMENT_3D('',#13191,#10456,#10457);
#8695=AXIS2_PLACEMENT_3D('',#13194,#10459,#10460);
#8696=AXIS2_PLACEMENT_3D('',#13195,#10461,#10462);
#8697=AXIS2_PLACEMENT_3D('',#13203,#10467,#10468);
#8698=AXIS2_PLACEMENT_3D('',#13206,#10470,#10471);
#8699=AXIS2_PLACEMENT_3D('',#13207,#10472,#10473);
#8700=AXIS2_PLACEMENT_3D('',#13211,#10476,#10477);
#8701=AXIS2_PLACEMENT_3D('',#13214,#10479,#10480);
#8702=AXIS2_PLACEMENT_3D('',#13215,#10481,#10482);
#8703=AXIS2_PLACEMENT_3D('',#13217,#10483,#10484);
#8704=AXIS2_PLACEMENT_3D('',#13219,#10485,#10486);
#8705=AXIS2_PLACEMENT_3D('',#13221,#10487,#10488);
#8706=AXIS2_PLACEMENT_3D('',#13222,#10489,#10490);
#8707=AXIS2_PLACEMENT_3D('',#13223,#10491,#10492);
#8708=AXIS2_PLACEMENT_3D('',#13226,#10493,#10494);
#8709=AXIS2_PLACEMENT_3D('',#13228,#10495,#10496);
#8710=AXIS2_PLACEMENT_3D('',#13229,#10497,#10498);
#8711=AXIS2_PLACEMENT_3D('',#13230,#10499,#10500);
#8712=AXIS2_PLACEMENT_3D('',#13233,#10501,#10502);
#8713=AXIS2_PLACEMENT_3D('',#13273,#10505,#10506);
#8714=AXIS2_PLACEMENT_3D('',#13328,#10507,#10508);
#8715=AXIS2_PLACEMENT_3D('',#13329,#10509,#10510);
#8716=AXIS2_PLACEMENT_3D('',#13330,#10511,#10512);
#8717=AXIS2_PLACEMENT_3D('',#13368,#10513,#10514);
#8718=AXIS2_PLACEMENT_3D('',#13379,#10515,#10516);
#8719=AXIS2_PLACEMENT_3D('',#13381,#10517,#10518);
#8720=AXIS2_PLACEMENT_3D('',#13384,#10521,#10522);
#8721=AXIS2_PLACEMENT_3D('',#13385,#10523,#10524);
#8722=AXIS2_PLACEMENT_3D('',#13386,#10525,#10526);
#8723=AXIS2_PLACEMENT_3D('',#13392,#10530,#10531);
#8724=AXIS2_PLACEMENT_3D('',#13395,#10533,#10534);
#8725=AXIS2_PLACEMENT_3D('',#13396,#10535,#10536);
#8726=AXIS2_PLACEMENT_3D('',#13404,#10541,#10542);
#8727=AXIS2_PLACEMENT_3D('',#13407,#10544,#10545);
#8728=AXIS2_PLACEMENT_3D('',#13408,#10546,#10547);
#8729=AXIS2_PLACEMENT_3D('',#13412,#10550,#10551);
#8730=AXIS2_PLACEMENT_3D('',#13415,#10553,#10554);
#8731=AXIS2_PLACEMENT_3D('',#13416,#10555,#10556);
#8732=AXIS2_PLACEMENT_3D('',#13417,#10557,#10558);
#8733=AXIS2_PLACEMENT_3D('',#13418,#10559,#10560);
#8734=AXIS2_PLACEMENT_3D('',#13419,#10561,#10562);
#8735=AXIS2_PLACEMENT_3D('',#13421,#10563,#10564);
#8736=AXIS2_PLACEMENT_3D('',#13434,#10566,#10567);
#8737=AXIS2_PLACEMENT_3D('',#13435,#10568,#10569);
#8738=AXIS2_PLACEMENT_3D('',#13436,#10570,#10571);
#8739=AXIS2_PLACEMENT_3D('',#13437,#10572,#10573);
#8740=AXIS2_PLACEMENT_3D('',#13440,#10574,#10575);
#8741=AXIS2_PLACEMENT_3D('',#13452,#10578,#10579);
#8742=AXIS2_PLACEMENT_3D('',#13453,#10580,#10581);
#8743=AXIS2_PLACEMENT_3D('',#13454,#10582,#10583);
#8744=AXIS2_PLACEMENT_3D('',#13456,#10584,#10585);
#8745=AXIS2_PLACEMENT_3D('',#13458,#10587,#10588);
#8746=AXIS2_PLACEMENT_3D('',#13460,#10590,#10591);
#8747=AXIS2_PLACEMENT_3D('',#13461,#10592,#10593);
#8748=AXIS2_PLACEMENT_3D('',#13463,#10594,#10595);
#8749=AXIS2_PLACEMENT_3D('',#13476,#10597,#10598);
#8750=AXIS2_PLACEMENT_3D('',#13477,#10599,#10600);
#8751=AXIS2_PLACEMENT_3D('',#13478,#10601,#10602);
#8752=AXIS2_PLACEMENT_3D('',#13479,#10603,#10604);
#8753=AXIS2_PLACEMENT_3D('',#13482,#10605,#10606);
#8754=AXIS2_PLACEMENT_3D('',#13494,#10609,#10610);
#8755=AXIS2_PLACEMENT_3D('',#13495,#10611,#10612);
#8756=AXIS2_PLACEMENT_3D('',#13496,#10613,#10614);
#8757=AXIS2_PLACEMENT_3D('',#13498,#10615,#10616);
#8758=AXIS2_PLACEMENT_3D('',#13500,#10618,#10619);
#8759=AXIS2_PLACEMENT_3D('',#13501,#10620,#10621);
#8760=AXIS2_PLACEMENT_3D('',#13503,#10622,#10623);
#8761=AXIS2_PLACEMENT_3D('',#13505,#10624,#10625);
#8762=AXIS2_PLACEMENT_3D('',#13507,#10627,#10628);
#8763=AXIS2_PLACEMENT_3D('',#13509,#10629,#10630);
#8764=AXIS2_PLACEMENT_3D('',#13510,#10631,#10632);
#8765=AXIS2_PLACEMENT_3D('',#13511,#10633,#10634);
#8766=AXIS2_PLACEMENT_3D('',#13524,#10636,#10637);
#8767=AXIS2_PLACEMENT_3D('',#13525,#10638,#10639);
#8768=AXIS2_PLACEMENT_3D('',#13526,#10640,#10641);
#8769=AXIS2_PLACEMENT_3D('',#13527,#10642,#10643);
#8770=AXIS2_PLACEMENT_3D('',#13529,#10644,#10645);
#8771=AXIS2_PLACEMENT_3D('',#13533,#10647,#10648);
#8772=AXIS2_PLACEMENT_3D('',#13541,#10652,#10653);
#8773=AXIS2_PLACEMENT_3D('',#13543,#10655,#10656);
#8774=AXIS2_PLACEMENT_3D('',#13544,#10657,#10658);
#8775=AXIS2_PLACEMENT_3D('',#13545,#10659,#10660);
#8776=AXIS2_PLACEMENT_3D('',#13546,#10661,#10662);
#8777=AXIS2_PLACEMENT_3D('',#13557,#10663,#10664);
#8778=AXIS2_PLACEMENT_3D('',#13558,#10665,#10666);
#8779=AXIS2_PLACEMENT_3D('',#13559,#10667,#10668);
#8780=AXIS2_PLACEMENT_3D('',#13561,#10669,#10670);
#8781=AXIS2_PLACEMENT_3D('',#13563,#10671,#10672);
#8782=AXIS2_PLACEMENT_3D('',#13565,#10674,#10675);
#8783=AXIS2_PLACEMENT_3D('',#13567,#10676,#10677);
#8784=AXIS2_PLACEMENT_3D('',#13568,#10678,#10679);
#8785=AXIS2_PLACEMENT_3D('',#13569,#10680,#10681);
#8786=AXIS2_PLACEMENT_3D('',#13582,#10683,#10684);
#8787=AXIS2_PLACEMENT_3D('',#13583,#10685,#10686);
#8788=AXIS2_PLACEMENT_3D('',#13584,#10687,#10688);
#8789=AXIS2_PLACEMENT_3D('',#13585,#10689,#10690);
#8790=AXIS2_PLACEMENT_3D('',#13587,#10691,#10692);
#8791=AXIS2_PLACEMENT_3D('',#13591,#10694,#10695);
#8792=AXIS2_PLACEMENT_3D('',#13600,#10700,#10701);
#8793=AXIS2_PLACEMENT_3D('',#13601,#10702,#10703);
#8794=AXIS2_PLACEMENT_3D('',#13602,#10704,#10705);
#8795=AXIS2_PLACEMENT_3D('',#13603,#10706,#10707);
#8796=AXIS2_PLACEMENT_3D('',#13604,#10708,#10709);
#8797=AXIS2_PLACEMENT_3D('',#13615,#10710,#10711);
#8798=AXIS2_PLACEMENT_3D('',#13616,#10712,#10713);
#8799=AXIS2_PLACEMENT_3D('',#13617,#10714,#10715);
#8800=AXIS2_PLACEMENT_3D('',#13619,#10717,#10718);
#8801=AXIS2_PLACEMENT_3D('',#13621,#10720,#10721);
#8802=AXIS2_PLACEMENT_3D('',#13627,#10725,#10726);
#8803=AXIS2_PLACEMENT_3D('',#13633,#10730,#10731);
#8804=AXIS2_PLACEMENT_3D('',#13637,#10733,#10734);
#8805=AXIS2_PLACEMENT_3D('',#13639,#10736,#10737);
#8806=AXIS2_PLACEMENT_3D('',#13641,#10739,#10740);
#8807=AXIS2_PLACEMENT_3D('',#13642,#10741,#10742);
#8808=AXIS2_PLACEMENT_3D('',#13648,#10746,#10747);
#8809=AXIS2_PLACEMENT_3D('',#13649,#10748,#10749);
#8810=AXIS2_PLACEMENT_3D('',#13650,#10750,#10751);
#8811=AXIS2_PLACEMENT_3D('',#13651,#10752,#10753);
#8812=AXIS2_PLACEMENT_3D('',#13652,#10754,#10755);
#8813=AXIS2_PLACEMENT_3D('',#13653,#10756,#10757);
#8814=AXIS2_PLACEMENT_3D('',#13654,#10758,#10759);
#8815=AXIS2_PLACEMENT_3D('',#13655,#10760,#10761);
#8816=AXIS2_PLACEMENT_3D('',#13656,#10762,#10763);
#8817=AXIS2_PLACEMENT_3D('',#13657,#10764,#10765);
#8818=AXIS2_PLACEMENT_3D('',#13658,#10766,#10767);
#8819=AXIS2_PLACEMENT_3D('',#13659,#10768,#10769);
#8820=AXIS2_PLACEMENT_3D('',#13662,#10771,#10772);
#8821=AXIS2_PLACEMENT_3D('',#13663,#10773,#10774);
#8822=AXIS2_PLACEMENT_3D('',#13667,#10777,#10778);
#8823=AXIS2_PLACEMENT_3D('',#13670,#10780,#10781);
#8824=AXIS2_PLACEMENT_3D('',#13671,#10782,#10783);
#8825=AXIS2_PLACEMENT_3D('',#13673,#10785,#10786);
#8826=AXIS2_PLACEMENT_3D('',#13674,#10787,#10788);
#8827=AXIS2_PLACEMENT_3D('',#13675,#10789,#10790);
#8828=AXIS2_PLACEMENT_3D('',#13677,#10791,#10792);
#8829=AXIS2_PLACEMENT_3D('',#13680,#10794,#10795);
#8830=AXIS2_PLACEMENT_3D('',#13681,#10796,#10797);
#8831=AXIS2_PLACEMENT_3D('',#13683,#10798,#10799);
#8832=AXIS2_PLACEMENT_3D('',#13685,#10801,#10802);
#8833=AXIS2_PLACEMENT_3D('',#13687,#10803,#10804);
#8834=AXIS2_PLACEMENT_3D('',#13688,#10805,#10806);
#8835=AXIS2_PLACEMENT_3D('',#13690,#10807,#10808);
#8836=AXIS2_PLACEMENT_3D('',#13692,#10810,#10811);
#8837=AXIS2_PLACEMENT_3D('',#13694,#10812,#10813);
#8838=AXIS2_PLACEMENT_3D('',#13695,#10814,#10815);
#8839=AXIS2_PLACEMENT_3D('',#13697,#10817,#10818);
#8840=AXIS2_PLACEMENT_3D('',#13737,#10819,#10820);
#8841=AXIS2_PLACEMENT_3D('',#13745,#10821,#10822);
#8842=AXIS2_PLACEMENT_3D('',#13785,#10823,#10824);
#8843=AXIS2_PLACEMENT_3D('',#13793,#10825,#10826);
#8844=AXIS2_PLACEMENT_3D('',#13794,#10827,#10828);
#8845=AXIS2_PLACEMENT_3D('',#13797,#10829,#10830);
#8846=AXIS2_PLACEMENT_3D('',#13832,#10833,#10834);
#8847=AXIS2_PLACEMENT_3D('',#13845,#10835,#10836);
#8848=AXIS2_PLACEMENT_3D('',#13848,#10837,#10838);
#8849=AXIS2_PLACEMENT_3D('',#13883,#10841,#10842);
#8850=AXIS2_PLACEMENT_3D('',#13896,#10843,#10844);
#8851=AXIS2_PLACEMENT_3D('',#13899,#10847,#10848);
#8852=AXIS2_PLACEMENT_3D('',#13902,#10851,#10852);
#8853=AXIS2_PLACEMENT_3D('',#13904,#10853,#10854);
#8854=AXIS2_PLACEMENT_3D('',#13905,#10855,#10856);
#8855=AXIS2_PLACEMENT_3D('',#13906,#10857,#10858);
#8856=AXIS2_PLACEMENT_3D('',#13907,#10859,#10860);
#8857=AXIS2_PLACEMENT_3D('',#13909,#10861,#10862);
#8858=AXIS2_PLACEMENT_3D('',#13912,#10864,#10865);
#8859=AXIS2_PLACEMENT_3D('',#13913,#10866,#10867);
#8860=AXIS2_PLACEMENT_3D('',#13915,#10868,#10869);
#8861=AXIS2_PLACEMENT_3D('',#13922,#10870,#10871);
#8862=AXIS2_PLACEMENT_3D('',#13924,#10872,#10873);
#8863=AXIS2_PLACEMENT_3D('',#13925,#10874,#10875);
#8864=AXIS2_PLACEMENT_3D('',#13965,#10876,#10877);
#8865=AXIS2_PLACEMENT_3D('',#13973,#10878,#10879);
#8866=AXIS2_PLACEMENT_3D('',#14013,#10880,#10881);
#8867=AXIS2_PLACEMENT_3D('',#14021,#10882,#10883);
#8868=AXIS2_PLACEMENT_3D('',#14022,#10884,#10885);
#8869=AXIS2_PLACEMENT_3D('',#14024,#10886,#10887);
#8870=AXIS2_PLACEMENT_3D('',#14058,#10890,#10891);
#8871=AXIS2_PLACEMENT_3D('',#14065,#10892,#10893);
#8872=AXIS2_PLACEMENT_3D('',#14067,#10894,#10895);
#8873=AXIS2_PLACEMENT_3D('',#14101,#10897,#10898);
#8874=AXIS2_PLACEMENT_3D('',#14114,#10899,#10900);
#8875=AXIS2_PLACEMENT_3D('',#14117,#10903,#10904);
#8876=AXIS2_PLACEMENT_3D('',#14118,#10905,#10906);
#8877=AXIS2_PLACEMENT_3D('',#14119,#10907,#10908);
#8878=AXIS2_PLACEMENT_3D('',#14120,#10909,#10910);
#8879=AXIS2_PLACEMENT_3D('',#14123,#10913,#10914);
#8880=AXIS2_PLACEMENT_3D('',#14124,#10915,#10916);
#8881=AXIS2_PLACEMENT_3D('',#14127,#10918,#10919);
#8882=AXIS2_PLACEMENT_3D('',#14128,#10920,#10921);
#8883=AXIS2_PLACEMENT_3D('',#14130,#10922,#10923);
#8884=AXIS2_PLACEMENT_3D('',#14131,#10924,#10925);
#8885=AXIS2_PLACEMENT_3D('',#14132,#10926,#10927);
#8886=AXIS2_PLACEMENT_3D('',#14133,#10928,#10929);
#8887=AXIS2_PLACEMENT_3D('',#14135,#10930,#10931);
#8888=AXIS2_PLACEMENT_3D('',#14136,#10932,#10933);
#8889=AXIS2_PLACEMENT_3D('',#14137,#10934,#10935);
#8890=AXIS2_PLACEMENT_3D('',#14139,#10936,#10937);
#8891=AXIS2_PLACEMENT_3D('',#14140,#10938,#10939);
#8892=AXIS2_PLACEMENT_3D('',#14142,#10940,#10941);
#8893=AXIS2_PLACEMENT_3D('',#14143,#10942,#10943);
#8894=AXIS2_PLACEMENT_3D('',#14144,#10944,#10945);
#8895=AXIS2_PLACEMENT_3D('',#14147,#10946,#10947);
#8896=AXIS2_PLACEMENT_3D('',#14149,#10949,#10950);
#8897=AXIS2_PLACEMENT_3D('',#14150,#10951,#10952);
#8898=AXIS2_PLACEMENT_3D('',#14152,#10953,#10954);
#8899=AXIS2_PLACEMENT_3D('',#14153,#10955,#10956);
#8900=AXIS2_PLACEMENT_3D('',#14154,#10957,#10958);
#8901=AXIS2_PLACEMENT_3D('',#14156,#10959,#10960);
#8902=AXIS2_PLACEMENT_3D('',#14157,#10961,#10962);
#8903=AXIS2_PLACEMENT_3D('',#14160,#10964,#10965);
#8904=AXIS2_PLACEMENT_3D('',#14161,#10966,#10967);
#8905=AXIS2_PLACEMENT_3D('',#14164,#10969,#10970);
#8906=AXIS2_PLACEMENT_3D('',#14165,#10971,#10972);
#8907=AXIS2_PLACEMENT_3D('',#14167,#10974,#10975);
#8908=AXIS2_PLACEMENT_3D('',#14168,#10976,#10977);
#8909=AXIS2_PLACEMENT_3D('',#14169,#10978,#10979);
#8910=AXIS2_PLACEMENT_3D('',#14191,#10981,#10982);
#8911=AXIS2_PLACEMENT_3D('',#14202,#10983,#10984);
#8912=AXIS2_PLACEMENT_3D('',#14292,#10986,#10987);
#8913=AXIS2_PLACEMENT_3D('',#14376,#10989,#10990);
#8914=AXIS2_PLACEMENT_3D('',#14466,#10992,#10993);
#8915=AXIS2_PLACEMENT_3D('',#14556,#10995,#10996);
#8916=AXIS2_PLACEMENT_3D('',#14646,#10998,#10999);
#8917=AXIS2_PLACEMENT_3D('',#14668,#11001,#11002);
#8918=AXIS2_PLACEMENT_3D('',#14682,#11003,#11004);
#8919=AXIS2_PLACEMENT_3D('',#14720,#11006,#11007);
#8920=AXIS2_PLACEMENT_3D('',#14758,#11009,#11010);
#8921=AXIS2_PLACEMENT_3D('',#14795,#11012,#11013);
#8922=AXIS2_PLACEMENT_3D('',#15420,#11015,#11016);
#8923=AXIS2_PLACEMENT_3D('',#15422,#11017,#11018);
#8924=AXIS2_PLACEMENT_3D('',#15998,#11019,#11020);
#8925=AXIS2_PLACEMENT_3D('',#16000,#11021,#11022);
#8926=AXIS2_PLACEMENT_3D('',#16001,#11023,#11024);
#8927=AXIS2_PLACEMENT_3D('',#16002,#11025,#11026);
#8928=AXIS2_PLACEMENT_3D('',#16004,#11027,#11028);
#8929=AXIS2_PLACEMENT_3D('',#16006,#11030,#11031);
#8930=AXIS2_PLACEMENT_3D('',#16008,#11032,#11033);
#8931=AXIS2_PLACEMENT_3D('',#16009,#11034,#11035);
#8932=AXIS2_PLACEMENT_3D('',#16011,#11036,#11037);
#8933=AXIS2_PLACEMENT_3D('',#16012,#11038,#11039);
#8934=AXIS2_PLACEMENT_3D('',#16014,#11041,#11042);
#8935=AXIS2_PLACEMENT_3D('',#16015,#11043,#11044);
#8936=AXIS2_PLACEMENT_3D('',#16043,#11045,#11046);
#8937=AXIS2_PLACEMENT_3D('',#16045,#11047,#11048);
#8938=AXIS2_PLACEMENT_3D('',#16046,#11049,#11050);
#8939=AXIS2_PLACEMENT_3D('',#16074,#11051,#11052);
#8940=AXIS2_PLACEMENT_3D('',#16076,#11053,#11054);
#8941=AXIS2_PLACEMENT_3D('',#16077,#11055,#11056);
#8942=AXIS2_PLACEMENT_3D('',#16105,#11057,#11058);
#8943=AXIS2_PLACEMENT_3D('',#16107,#11059,#11060);
#8944=AXIS2_PLACEMENT_3D('',#16108,#11061,#11062);
#8945=AXIS2_PLACEMENT_3D('',#16136,#11063,#11064);
#8946=AXIS2_PLACEMENT_3D('',#16138,#11065,#11066);
#8947=AXIS2_PLACEMENT_3D('',#16139,#11067,#11068);
#8948=AXIS2_PLACEMENT_3D('',#16140,#11069,#11070);
#8949=AXIS2_PLACEMENT_3D('',#16143,#11073,#11074);
#8950=AXIS2_PLACEMENT_3D('',#16146,#11077,#11078);
#8951=AXIS2_PLACEMENT_3D('',#16149,#11081,#11082);
#8952=AXIS2_PLACEMENT_3D('',#16152,#11085,#11086);
#8953=AXIS2_PLACEMENT_3D('',#16158,#11090,#11091);
#8954=AXIS2_PLACEMENT_3D('',#16161,#11093,#11094);
#8955=AXIS2_PLACEMENT_3D('',#16162,#11095,#11096);
#8956=AXIS2_PLACEMENT_3D('',#16166,#11099,#11100);
#8957=AXIS2_PLACEMENT_3D('',#16169,#11102,#11103);
#8958=AXIS2_PLACEMENT_3D('',#16170,#11104,#11105);
#8959=AXIS2_PLACEMENT_3D('',#16173,#11106,#11107);
#8960=AXIS2_PLACEMENT_3D('',#16175,#11108,#11109);
#8961=AXIS2_PLACEMENT_3D('',#16177,#11110,#11111);
#8962=AXIS2_PLACEMENT_3D('',#16178,#11112,#11113);
#8963=AXIS2_PLACEMENT_3D('',#16179,#11114,#11115);
#8964=AXIS2_PLACEMENT_3D('',#16188,#11120,#11121);
#8965=AXIS2_PLACEMENT_3D('',#16190,#11122,#11123);
#8966=AXIS2_PLACEMENT_3D('',#16193,#11125,#11126);
#8967=AXIS2_PLACEMENT_3D('',#16194,#11127,#11128);
#8968=AXIS2_PLACEMENT_3D('',#16200,#11132,#11133);
#8969=AXIS2_PLACEMENT_3D('',#16202,#11134,#11135);
#8970=AXIS2_PLACEMENT_3D('',#16205,#11137,#11138);
#8971=AXIS2_PLACEMENT_3D('',#16206,#11139,#11140);
#8972=AXIS2_PLACEMENT_3D('',#16208,#11141,#11142);
#8973=AXIS2_PLACEMENT_3D('',#16210,#11143,#11144);
#8974=AXIS2_PLACEMENT_3D('',#16212,#11146,#11147);
#8975=AXIS2_PLACEMENT_3D('',#16218,#11151,#11152);
#8976=AXIS2_PLACEMENT_3D('',#16220,#11153,#11154);
#8977=AXIS2_PLACEMENT_3D('',#16222,#11155,#11156);
#8978=AXIS2_PLACEMENT_3D('',#16224,#11158,#11159);
#8979=AXIS2_PLACEMENT_3D('',#16227,#11162,#11163);
#8980=AXIS2_PLACEMENT_3D('',#16230,#11164,#11165);
#8981=AXIS2_PLACEMENT_3D('',#16232,#11166,#11167);
#8982=AXIS2_PLACEMENT_3D('',#16234,#11168,#11169);
#8983=AXIS2_PLACEMENT_3D('',#16235,#11170,#11171);
#8984=AXIS2_PLACEMENT_3D('',#16236,#11172,#11173);
#8985=AXIS2_PLACEMENT_3D('',#16240,#11175,#11176);
#8986=AXIS2_PLACEMENT_3D('',#16243,#11178,#11179);
#8987=AXIS2_PLACEMENT_3D('',#16244,#11180,#11181);
#8988=AXIS2_PLACEMENT_3D('',#16247,#11184,#11185);
#8989=AXIS2_PLACEMENT_3D('',#16249,#11187,#11188);
#8990=AXIS2_PLACEMENT_3D('',#16251,#11190,#11191);
#8991=AXIS2_PLACEMENT_3D('',#16252,#11192,#11193);
#8992=AXIS2_PLACEMENT_3D('',#16255,#11196,#11197);
#8993=AXIS2_PLACEMENT_3D('',#16256,#11198,#11199);
#8994=AXIS2_PLACEMENT_3D('',#16258,#11201,#11202);
#8995=AXIS2_PLACEMENT_3D('',#16259,#11203,#11204);
#8996=AXIS2_PLACEMENT_3D('',#16260,#11205,#11206);
#8997=AXIS2_PLACEMENT_3D('',#16281,#11208,#11209);
#8998=AXIS2_PLACEMENT_3D('',#16283,#11210,#11211);
#8999=AXIS2_PLACEMENT_3D('',#16285,#11212,#11213);
#9000=AXIS2_PLACEMENT_3D('',#16287,#11215,#11216);
#9001=AXIS2_PLACEMENT_3D('',#16289,#11217,#11218);
#9002=AXIS2_PLACEMENT_3D('',#16291,#11220,#11221);
#9003=AXIS2_PLACEMENT_3D('',#16293,#11222,#11223);
#9004=AXIS2_PLACEMENT_3D('',#16297,#11225,#11226);
#9005=AXIS2_PLACEMENT_3D('',#16299,#11228,#11229);
#9006=AXIS2_PLACEMENT_3D('',#16301,#11230,#11231);
#9007=AXIS2_PLACEMENT_3D('',#16303,#11233,#11234);
#9008=AXIS2_PLACEMENT_3D('',#16321,#11235,#11236);
#9009=AXIS2_PLACEMENT_3D('',#16323,#11237,#11238);
#9010=AXIS2_PLACEMENT_3D('',#16325,#11240,#11241);
#9011=AXIS2_PLACEMENT_3D('',#16327,#11242,#11243);
#9012=AXIS2_PLACEMENT_3D('',#16329,#11245,#11246);
#9013=AXIS2_PLACEMENT_3D('',#16331,#11247,#11248);
#9014=AXIS2_PLACEMENT_3D('',#16335,#11250,#11251);
#9015=AXIS2_PLACEMENT_3D('',#16337,#11253,#11254);
#9016=AXIS2_PLACEMENT_3D('',#16339,#11255,#11256);
#9017=AXIS2_PLACEMENT_3D('',#16341,#11258,#11259);
#9018=AXIS2_PLACEMENT_3D('',#16362,#11261,#11262);
#9019=AXIS2_PLACEMENT_3D('',#16364,#11263,#11264);
#9020=AXIS2_PLACEMENT_3D('',#16366,#11265,#11266);
#9021=AXIS2_PLACEMENT_3D('',#16368,#11268,#11269);
#9022=AXIS2_PLACEMENT_3D('',#16370,#11270,#11271);
#9023=AXIS2_PLACEMENT_3D('',#16372,#11273,#11274);
#9024=AXIS2_PLACEMENT_3D('',#16390,#11275,#11276);
#9025=AXIS2_PLACEMENT_3D('',#16392,#11277,#11278);
#9026=AXIS2_PLACEMENT_3D('',#16394,#11280,#11281);
#9027=AXIS2_PLACEMENT_3D('',#16396,#11282,#11283);
#9028=AXIS2_PLACEMENT_3D('',#16398,#11285,#11286);
#9029=AXIS2_PLACEMENT_3D('',#16400,#11287,#11288);
#9030=AXIS2_PLACEMENT_3D('',#16402,#11290,#11291);
#9031=AXIS2_PLACEMENT_3D('',#16404,#11292,#11293);
#9032=AXIS2_PLACEMENT_3D('',#16406,#11295,#11296);
#9033=AXIS2_PLACEMENT_3D('',#16407,#11297,#11298);
#9034=AXIS2_PLACEMENT_3D('',#16409,#11299,#11300);
#9035=AXIS2_PLACEMENT_3D('',#16411,#11302,#11303);
#9036=AXIS2_PLACEMENT_3D('',#16412,#11304,#11305);
#9037=AXIS2_PLACEMENT_3D('',#16414,#11307,#11308);
#9038=AXIS2_PLACEMENT_3D('',#16415,#11309,#11310);
#9039=AXIS2_PLACEMENT_3D('',#16417,#11311,#11312);
#9040=AXIS2_PLACEMENT_3D('',#16419,#11313,#11314);
#9041=AXIS2_PLACEMENT_3D('',#16420,#11315,#11316);
#9042=AXIS2_PLACEMENT_3D('',#16421,#11317,#11318);
#9043=AXIS2_PLACEMENT_3D('',#16423,#11319,#11320);
#9044=AXIS2_PLACEMENT_3D('',#16424,#11321,#11322);
#9045=AXIS2_PLACEMENT_3D('',#16426,#11323,#11324);
#9046=AXIS2_PLACEMENT_3D('',#16428,#11326,#11327);
#9047=AXIS2_PLACEMENT_3D('',#16430,#11328,#11329);
#9048=AXIS2_PLACEMENT_3D('',#16432,#11331,#11332);
#9049=AXIS2_PLACEMENT_3D('',#16434,#11333,#11334);
#9050=AXIS2_PLACEMENT_3D('',#16436,#11336,#11337);
#9051=AXIS2_PLACEMENT_3D('',#16437,#11338,#11339);
#9052=AXIS2_PLACEMENT_3D('',#16439,#11340,#11341);
#9053=AXIS2_PLACEMENT_3D('',#16441,#11342,#11343);
#9054=AXIS2_PLACEMENT_3D('',#16442,#11344,#11345);
#9055=AXIS2_PLACEMENT_3D('',#16443,#11346,#11347);
#9056=AXIS2_PLACEMENT_3D('',#16445,#11349,#11350);
#9057=AXIS2_PLACEMENT_3D('',#16446,#11351,#11352);
#9058=AXIS2_PLACEMENT_3D('',#16467,#11354,#11355);
#9059=AXIS2_PLACEMENT_3D('',#16469,#11356,#11357);
#9060=AXIS2_PLACEMENT_3D('',#16471,#11358,#11359);
#9061=AXIS2_PLACEMENT_3D('',#16473,#11361,#11362);
#9062=AXIS2_PLACEMENT_3D('',#16475,#11363,#11364);
#9063=AXIS2_PLACEMENT_3D('',#16477,#11366,#11367);
#9064=AXIS2_PLACEMENT_3D('',#16479,#11368,#11369);
#9065=AXIS2_PLACEMENT_3D('',#16483,#11371,#11372);
#9066=AXIS2_PLACEMENT_3D('',#16485,#11374,#11375);
#9067=AXIS2_PLACEMENT_3D('',#16487,#11376,#11377);
#9068=AXIS2_PLACEMENT_3D('',#16489,#11379,#11380);
#9069=AXIS2_PLACEMENT_3D('',#16507,#11381,#11382);
#9070=AXIS2_PLACEMENT_3D('',#16509,#11383,#11384);
#9071=AXIS2_PLACEMENT_3D('',#16511,#11386,#11387);
#9072=AXIS2_PLACEMENT_3D('',#16513,#11388,#11389);
#9073=AXIS2_PLACEMENT_3D('',#16515,#11391,#11392);
#9074=AXIS2_PLACEMENT_3D('',#16517,#11393,#11394);
#9075=AXIS2_PLACEMENT_3D('',#16521,#11396,#11397);
#9076=AXIS2_PLACEMENT_3D('',#16523,#11399,#11400);
#9077=AXIS2_PLACEMENT_3D('',#16525,#11401,#11402);
#9078=AXIS2_PLACEMENT_3D('',#16527,#11404,#11405);
#9079=AXIS2_PLACEMENT_3D('',#16548,#11407,#11408);
#9080=AXIS2_PLACEMENT_3D('',#16550,#11409,#11410);
#9081=AXIS2_PLACEMENT_3D('',#16552,#11411,#11412);
#9082=AXIS2_PLACEMENT_3D('',#16554,#11414,#11415);
#9083=AXIS2_PLACEMENT_3D('',#16556,#11416,#11417);
#9084=AXIS2_PLACEMENT_3D('',#16558,#11419,#11420);
#9085=AXIS2_PLACEMENT_3D('',#16576,#11421,#11422);
#9086=AXIS2_PLACEMENT_3D('',#16578,#11423,#11424);
#9087=AXIS2_PLACEMENT_3D('',#16580,#11426,#11427);
#9088=AXIS2_PLACEMENT_3D('',#16582,#11428,#11429);
#9089=AXIS2_PLACEMENT_3D('',#16584,#11431,#11432);
#9090=AXIS2_PLACEMENT_3D('',#16586,#11433,#11434);
#9091=AXIS2_PLACEMENT_3D('',#16588,#11436,#11437);
#9092=AXIS2_PLACEMENT_3D('',#16590,#11438,#11439);
#9093=AXIS2_PLACEMENT_3D('',#16592,#11441,#11442);
#9094=AXIS2_PLACEMENT_3D('',#16593,#11443,#11444);
#9095=AXIS2_PLACEMENT_3D('',#16595,#11445,#11446);
#9096=AXIS2_PLACEMENT_3D('',#16597,#11448,#11449);
#9097=AXIS2_PLACEMENT_3D('',#16598,#11450,#11451);
#9098=AXIS2_PLACEMENT_3D('',#16600,#11453,#11454);
#9099=AXIS2_PLACEMENT_3D('',#16601,#11455,#11456);
#9100=AXIS2_PLACEMENT_3D('',#16603,#11457,#11458);
#9101=AXIS2_PLACEMENT_3D('',#16605,#11459,#11460);
#9102=AXIS2_PLACEMENT_3D('',#16606,#11461,#11462);
#9103=AXIS2_PLACEMENT_3D('',#16607,#11463,#11464);
#9104=AXIS2_PLACEMENT_3D('',#16609,#11465,#11466);
#9105=AXIS2_PLACEMENT_3D('',#16610,#11467,#11468);
#9106=AXIS2_PLACEMENT_3D('',#16612,#11469,#11470);
#9107=AXIS2_PLACEMENT_3D('',#16614,#11472,#11473);
#9108=AXIS2_PLACEMENT_3D('',#16616,#11474,#11475);
#9109=AXIS2_PLACEMENT_3D('',#16618,#11477,#11478);
#9110=AXIS2_PLACEMENT_3D('',#16620,#11479,#11480);
#9111=AXIS2_PLACEMENT_3D('',#16622,#11482,#11483);
#9112=AXIS2_PLACEMENT_3D('',#16623,#11484,#11485);
#9113=AXIS2_PLACEMENT_3D('',#16625,#11486,#11487);
#9114=AXIS2_PLACEMENT_3D('',#16627,#11488,#11489);
#9115=AXIS2_PLACEMENT_3D('',#16628,#11490,#11491);
#9116=AXIS2_PLACEMENT_3D('',#16629,#11492,#11493);
#9117=AXIS2_PLACEMENT_3D('',#16631,#11495,#11496);
#9118=AXIS2_PLACEMENT_3D('',#16632,#11497,#11498);
#9119=AXIS2_PLACEMENT_3D('',#16653,#11500,#11501);
#9120=AXIS2_PLACEMENT_3D('',#16655,#11502,#11503);
#9121=AXIS2_PLACEMENT_3D('',#16657,#11504,#11505);
#9122=AXIS2_PLACEMENT_3D('',#16659,#11507,#11508);
#9123=AXIS2_PLACEMENT_3D('',#16661,#11509,#11510);
#9124=AXIS2_PLACEMENT_3D('',#16663,#11512,#11513);
#9125=AXIS2_PLACEMENT_3D('',#16665,#11514,#11515);
#9126=AXIS2_PLACEMENT_3D('',#16669,#11517,#11518);
#9127=AXIS2_PLACEMENT_3D('',#16671,#11520,#11521);
#9128=AXIS2_PLACEMENT_3D('',#16673,#11522,#11523);
#9129=AXIS2_PLACEMENT_3D('',#16675,#11525,#11526);
#9130=AXIS2_PLACEMENT_3D('',#16693,#11527,#11528);
#9131=AXIS2_PLACEMENT_3D('',#16695,#11529,#11530);
#9132=AXIS2_PLACEMENT_3D('',#16697,#11532,#11533);
#9133=AXIS2_PLACEMENT_3D('',#16699,#11534,#11535);
#9134=AXIS2_PLACEMENT_3D('',#16701,#11537,#11538);
#9135=AXIS2_PLACEMENT_3D('',#16703,#11539,#11540);
#9136=AXIS2_PLACEMENT_3D('',#16707,#11542,#11543);
#9137=AXIS2_PLACEMENT_3D('',#16709,#11545,#11546);
#9138=AXIS2_PLACEMENT_3D('',#16711,#11547,#11548);
#9139=AXIS2_PLACEMENT_3D('',#16713,#11550,#11551);
#9140=AXIS2_PLACEMENT_3D('',#16734,#11553,#11554);
#9141=AXIS2_PLACEMENT_3D('',#16736,#11555,#11556);
#9142=AXIS2_PLACEMENT_3D('',#16738,#11557,#11558);
#9143=AXIS2_PLACEMENT_3D('',#16740,#11560,#11561);
#9144=AXIS2_PLACEMENT_3D('',#16742,#11562,#11563);
#9145=AXIS2_PLACEMENT_3D('',#16744,#11565,#11566);
#9146=AXIS2_PLACEMENT_3D('',#16762,#11567,#11568);
#9147=AXIS2_PLACEMENT_3D('',#16764,#11569,#11570);
#9148=AXIS2_PLACEMENT_3D('',#16766,#11572,#11573);
#9149=AXIS2_PLACEMENT_3D('',#16768,#11574,#11575);
#9150=AXIS2_PLACEMENT_3D('',#16770,#11577,#11578);
#9151=AXIS2_PLACEMENT_3D('',#16772,#11579,#11580);
#9152=AXIS2_PLACEMENT_3D('',#16774,#11582,#11583);
#9153=AXIS2_PLACEMENT_3D('',#16776,#11584,#11585);
#9154=AXIS2_PLACEMENT_3D('',#16778,#11587,#11588);
#9155=AXIS2_PLACEMENT_3D('',#16779,#11589,#11590);
#9156=AXIS2_PLACEMENT_3D('',#16781,#11591,#11592);
#9157=AXIS2_PLACEMENT_3D('',#16783,#11594,#11595);
#9158=AXIS2_PLACEMENT_3D('',#16784,#11596,#11597);
#9159=AXIS2_PLACEMENT_3D('',#16786,#11599,#11600);
#9160=AXIS2_PLACEMENT_3D('',#16787,#11601,#11602);
#9161=AXIS2_PLACEMENT_3D('',#16789,#11603,#11604);
#9162=AXIS2_PLACEMENT_3D('',#16791,#11605,#11606);
#9163=AXIS2_PLACEMENT_3D('',#16792,#11607,#11608);
#9164=AXIS2_PLACEMENT_3D('',#16793,#11609,#11610);
#9165=AXIS2_PLACEMENT_3D('',#16795,#11611,#11612);
#9166=AXIS2_PLACEMENT_3D('',#16796,#11613,#11614);
#9167=AXIS2_PLACEMENT_3D('',#16798,#11615,#11616);
#9168=AXIS2_PLACEMENT_3D('',#16800,#11618,#11619);
#9169=AXIS2_PLACEMENT_3D('',#16802,#11620,#11621);
#9170=AXIS2_PLACEMENT_3D('',#16804,#11623,#11624);
#9171=AXIS2_PLACEMENT_3D('',#16806,#11625,#11626);
#9172=AXIS2_PLACEMENT_3D('',#16808,#11628,#11629);
#9173=AXIS2_PLACEMENT_3D('',#16809,#11630,#11631);
#9174=AXIS2_PLACEMENT_3D('',#16811,#11632,#11633);
#9175=AXIS2_PLACEMENT_3D('',#16813,#11634,#11635);
#9176=AXIS2_PLACEMENT_3D('',#16814,#11636,#11637);
#9177=AXIS2_PLACEMENT_3D('',#16815,#11638,#11639);
#9178=AXIS2_PLACEMENT_3D('',#16817,#11641,#11642);
#9179=AXIS2_PLACEMENT_3D('',#16818,#11643,#11644);
#9180=AXIS2_PLACEMENT_3D('',#16839,#11646,#11647);
#9181=AXIS2_PLACEMENT_3D('',#16841,#11648,#11649);
#9182=AXIS2_PLACEMENT_3D('',#16843,#11650,#11651);
#9183=AXIS2_PLACEMENT_3D('',#16845,#11653,#11654);
#9184=AXIS2_PLACEMENT_3D('',#16847,#11655,#11656);
#9185=AXIS2_PLACEMENT_3D('',#16849,#11658,#11659);
#9186=AXIS2_PLACEMENT_3D('',#16851,#11660,#11661);
#9187=AXIS2_PLACEMENT_3D('',#16855,#11663,#11664);
#9188=AXIS2_PLACEMENT_3D('',#16857,#11666,#11667);
#9189=AXIS2_PLACEMENT_3D('',#16859,#11668,#11669);
#9190=AXIS2_PLACEMENT_3D('',#16861,#11671,#11672);
#9191=AXIS2_PLACEMENT_3D('',#16879,#11673,#11674);
#9192=AXIS2_PLACEMENT_3D('',#16881,#11675,#11676);
#9193=AXIS2_PLACEMENT_3D('',#16883,#11678,#11679);
#9194=AXIS2_PLACEMENT_3D('',#16885,#11680,#11681);
#9195=AXIS2_PLACEMENT_3D('',#16887,#11683,#11684);
#9196=AXIS2_PLACEMENT_3D('',#16889,#11685,#11686);
#9197=AXIS2_PLACEMENT_3D('',#16893,#11688,#11689);
#9198=AXIS2_PLACEMENT_3D('',#16895,#11691,#11692);
#9199=AXIS2_PLACEMENT_3D('',#16897,#11693,#11694);
#9200=AXIS2_PLACEMENT_3D('',#16899,#11696,#11697);
#9201=AXIS2_PLACEMENT_3D('',#16920,#11699,#11700);
#9202=AXIS2_PLACEMENT_3D('',#16922,#11701,#11702);
#9203=AXIS2_PLACEMENT_3D('',#16924,#11703,#11704);
#9204=AXIS2_PLACEMENT_3D('',#16926,#11706,#11707);
#9205=AXIS2_PLACEMENT_3D('',#16928,#11708,#11709);
#9206=AXIS2_PLACEMENT_3D('',#16930,#11711,#11712);
#9207=AXIS2_PLACEMENT_3D('',#16948,#11713,#11714);
#9208=AXIS2_PLACEMENT_3D('',#16950,#11715,#11716);
#9209=AXIS2_PLACEMENT_3D('',#16952,#11718,#11719);
#9210=AXIS2_PLACEMENT_3D('',#16954,#11720,#11721);
#9211=AXIS2_PLACEMENT_3D('',#16956,#11723,#11724);
#9212=AXIS2_PLACEMENT_3D('',#16958,#11725,#11726);
#9213=AXIS2_PLACEMENT_3D('',#16960,#11728,#11729);
#9214=AXIS2_PLACEMENT_3D('',#16962,#11730,#11731);
#9215=AXIS2_PLACEMENT_3D('',#16964,#11733,#11734);
#9216=AXIS2_PLACEMENT_3D('',#16965,#11735,#11736);
#9217=AXIS2_PLACEMENT_3D('',#16967,#11737,#11738);
#9218=AXIS2_PLACEMENT_3D('',#16969,#11740,#11741);
#9219=AXIS2_PLACEMENT_3D('',#16970,#11742,#11743);
#9220=AXIS2_PLACEMENT_3D('',#16972,#11745,#11746);
#9221=AXIS2_PLACEMENT_3D('',#16973,#11747,#11748);
#9222=AXIS2_PLACEMENT_3D('',#16975,#11749,#11750);
#9223=AXIS2_PLACEMENT_3D('',#16977,#11751,#11752);
#9224=AXIS2_PLACEMENT_3D('',#16978,#11753,#11754);
#9225=AXIS2_PLACEMENT_3D('',#16979,#11755,#11756);
#9226=AXIS2_PLACEMENT_3D('',#16981,#11757,#11758);
#9227=AXIS2_PLACEMENT_3D('',#16982,#11759,#11760);
#9228=AXIS2_PLACEMENT_3D('',#16984,#11761,#11762);
#9229=AXIS2_PLACEMENT_3D('',#16986,#11764,#11765);
#9230=AXIS2_PLACEMENT_3D('',#16988,#11766,#11767);
#9231=AXIS2_PLACEMENT_3D('',#16990,#11769,#11770);
#9232=AXIS2_PLACEMENT_3D('',#16992,#11771,#11772);
#9233=AXIS2_PLACEMENT_3D('',#16994,#11774,#11775);
#9234=AXIS2_PLACEMENT_3D('',#16995,#11776,#11777);
#9235=AXIS2_PLACEMENT_3D('',#16997,#11778,#11779);
#9236=AXIS2_PLACEMENT_3D('',#16999,#11780,#11781);
#9237=AXIS2_PLACEMENT_3D('',#17000,#11782,#11783);
#9238=AXIS2_PLACEMENT_3D('',#17001,#11784,#11785);
#9239=AXIS2_PLACEMENT_3D('',#17003,#11787,#11788);
#9240=AXIS2_PLACEMENT_3D('',#17004,#11789,#11790);
#9241=AXIS2_PLACEMENT_3D('',#17005,#11791,#11792);
#9242=AXIS2_PLACEMENT_3D('',#17006,#11793,#11794);
#9243=AXIS2_PLACEMENT_3D('',#17007,#11795,#11796);
#9244=AXIS2_PLACEMENT_3D('',#17008,#11797,#11798);
#9245=AXIS2_PLACEMENT_3D('',#17009,#11799,#11800);
#9246=AXIS2_PLACEMENT_3D('',#17010,#11801,#11802);
#9247=AXIS2_PLACEMENT_3D('',#17011,#11803,#11804);
#9248=AXIS2_PLACEMENT_3D('',#17012,#11805,#11806);
#9249=AXIS2_PLACEMENT_3D('',#17013,#11807,#11808);
#9250=AXIS2_PLACEMENT_3D('',#17014,#11809,#11810);
#9251=DIRECTION('axis',(0.,0.,1.));
#9252=DIRECTION('refdir',(1.,0.,0.));
#9253=DIRECTION('axis',(0.,0.,1.));
#9254=DIRECTION('refdir',(1.,0.,0.));
#9255=DIRECTION('center_axis',(-1.,0.,0.));
#9256=DIRECTION('ref_axis',(0.,0.,1.));
#9257=DIRECTION('',(1.,0.,0.));
#9258=DIRECTION('center_axis',(1.,-9.61038138866416E-16,0.));
#9259=DIRECTION('ref_axis',(0.,0.,1.));
#9260=DIRECTION('',(-1.,0.,0.));
#9261=DIRECTION('center_axis',(1.,0.,0.));
#9262=DIRECTION('ref_axis',(0.,0.,1.));
#9263=DIRECTION('',(-1.,0.,0.));
#9264=DIRECTION('center_axis',(-1.,0.,0.));
#9265=DIRECTION('ref_axis',(0.,0.,1.));
#9266=DIRECTION('center_axis',(0.,-1.,0.));
#9267=DIRECTION('ref_axis',(0.,0.,1.));
#9268=DIRECTION('',(0.,0.,-1.));
#9269=DIRECTION('',(1.,0.,0.));
#9270=DIRECTION('',(0.,0.,-1.));
#9271=DIRECTION('center_axis',(0.,1.,0.));
#9272=DIRECTION('ref_axis',(-1.,0.,0.));
#9273=DIRECTION('',(0.,0.,1.));
#9274=DIRECTION('',(-1.,0.,0.));
#9275=DIRECTION('',(0.,0.,1.));
#9276=DIRECTION('',(0.,0.,1.));
#9277=DIRECTION('',(1.,0.,0.));
#9278=DIRECTION('center_axis',(0.,0.,1.));
#9279=DIRECTION('ref_axis',(-2.22044604925031E-15,1.,0.));
#9280=DIRECTION('center_axis',(0.,0.,1.));
#9281=DIRECTION('ref_axis',(-2.22044604925031E-15,1.,0.));
#9282=DIRECTION('',(0.,0.,1.));
#9283=DIRECTION('center_axis',(1.,0.,0.));
#9284=DIRECTION('ref_axis',(0.,1.,0.));
#9285=DIRECTION('',(0.,1.,0.));
#9286=DIRECTION('',(0.,0.,1.));
#9287=DIRECTION('',(0.,-1.,0.));
#9288=DIRECTION('center_axis',(0.,0.,1.));
#9289=DIRECTION('ref_axis',(1.,2.22044604925032E-15,0.));
#9290=DIRECTION('center_axis',(0.,0.,1.));
#9291=DIRECTION('ref_axis',(1.,2.22044604925032E-15,0.));
#9292=DIRECTION('',(0.,0.,1.));
#9293=DIRECTION('center_axis',(0.,0.,-1.));
#9294=DIRECTION('ref_axis',(1.,2.22044604925032E-15,0.));
#9295=DIRECTION('center_axis',(0.,-1.,0.));
#9296=DIRECTION('ref_axis',(1.,0.,0.));
#9297=DIRECTION('',(0.,0.,-1.));
#9298=DIRECTION('',(-1.,0.,0.));
#9299=DIRECTION('',(1.,0.,0.));
#9300=DIRECTION('center_axis',(0.,0.,-1.));
#9301=DIRECTION('ref_axis',(0.,1.,0.));
#9302=DIRECTION('',(0.,1.,0.));
#9303=DIRECTION('',(-1.,0.,0.));
#9304=DIRECTION('',(0.,1.,0.));
#9305=DIRECTION('center_axis',(0.,0.,-1.));
#9306=DIRECTION('ref_axis',(0.,1.,0.));
#9307=DIRECTION('',(0.,1.,0.));
#9308=DIRECTION('',(1.,0.,0.));
#9309=DIRECTION('',(0.,1.,0.));
#9310=DIRECTION('',(-1.,0.,0.));
#9311=DIRECTION('',(0.,1.,0.));
#9312=DIRECTION('center_axis',(1.,0.,0.));
#9313=DIRECTION('ref_axis',(0.,1.,0.));
#9314=DIRECTION('',(0.,1.,0.));
#9315=DIRECTION('center_axis',(1.,0.,0.));
#9316=DIRECTION('ref_axis',(0.,-1.,0.));
#9317=DIRECTION('',(0.,0.,-1.));
#9318=DIRECTION('center_axis',(1.,0.,0.));
#9319=DIRECTION('ref_axis',(0.,-0.707106781186549,0.707106781186546));
#9320=DIRECTION('',(0.,-1.,0.));
#9321=DIRECTION('',(0.,0.,-1.));
#9322=DIRECTION('',(0.,-1.,0.));
#9323=DIRECTION('',(0.,0.,-1.));
#9324=DIRECTION('center_axis',(1.,0.,0.));
#9325=DIRECTION('ref_axis',(0.,1.,0.));
#9326=DIRECTION('center_axis',(1.,0.,0.));
#9327=DIRECTION('ref_axis',(0.,1.,0.));
#9328=DIRECTION('',(0.,0.,-1.));
#9329=DIRECTION('center_axis',(1.,0.,0.));
#9330=DIRECTION('ref_axis',(0.,1.,0.));
#9331=DIRECTION('center_axis',(1.,0.,0.));
#9332=DIRECTION('ref_axis',(0.,1.,0.));
#9333=DIRECTION('center_axis',(1.,0.,0.));
#9334=DIRECTION('ref_axis',(0.,-0.707106781186548,-0.707106781186547));
#9335=DIRECTION('center_axis',(-1.,0.,0.));
#9336=DIRECTION('ref_axis',(0.,0.,-1.));
#9337=DIRECTION('',(-1.,0.,0.));
#9338=DIRECTION('center_axis',(-1.,0.,0.));
#9339=DIRECTION('ref_axis',(0.,-0.707106781186548,-0.707106781186547));
#9340=DIRECTION('',(1.,0.,0.));
#9341=DIRECTION('center_axis',(0.,0.,1.));
#9342=DIRECTION('ref_axis',(0.707106781186548,0.707106781186548,0.));
#9343=DIRECTION('',(0.,0.,1.));
#9344=DIRECTION('center_axis',(0.,-5.55111512312576E-16,-1.));
#9345=DIRECTION('ref_axis',(0.,1.,-5.55111512312577E-16));
#9346=DIRECTION('',(0.,0.,-1.));
#9347=DIRECTION('center_axis',(0.,0.707106781186548,0.707106781186548));
#9348=DIRECTION('ref_axis',(0.,0.707106781186548,-0.707106781186548));
#9349=DIRECTION('center_axis',(0.,1.,0.));
#9350=DIRECTION('ref_axis',(0.707106781186548,0.,-0.707106781186548));
#9351=DIRECTION('',(0.,-1.,0.));
#9352=DIRECTION('center_axis',(0.,0.707106781186548,-0.707106781186547));
#9353=DIRECTION('ref_axis',(0.,-0.707106781186547,-0.707106781186548));
#9354=DIRECTION('',(0.,1.,0.));
#9355=DIRECTION('center_axis',(0.,1.,0.));
#9356=DIRECTION('ref_axis',(0.707106781186548,0.,-0.707106781186547));
#9357=DIRECTION('center_axis',(0.,1.,0.));
#9358=DIRECTION('ref_axis',(1.,0.,0.));
#9359=DIRECTION('',(0.,1.,0.));
#9360=DIRECTION('center_axis',(0.,-1.,0.));
#9361=DIRECTION('ref_axis',(0.,0.,-1.));
#9362=DIRECTION('',(0.,-1.,0.));
#9363=DIRECTION('center_axis',(-1.,0.,0.));
#9364=DIRECTION('ref_axis',(0.,0.,1.));
#9365=DIRECTION('center_axis',(0.,-5.55111512312578E-16,1.));
#9366=DIRECTION('ref_axis',(0.,-1.,-5.55111512312578E-16));
#9367=DIRECTION('center_axis',(1.,0.,0.));
#9368=DIRECTION('ref_axis',(0.,0.707106781186548,0.707106781186548));
#9369=DIRECTION('center_axis',(-1.,0.,0.));
#9370=DIRECTION('ref_axis',(0.,0.707106781186548,0.707106781186548));
#9371=DIRECTION('center_axis',(0.,0.,-1.));
#9372=DIRECTION('ref_axis',(0.707106781186548,-0.707106781186548,0.));
#9373=DIRECTION('',(0.,0.,1.));
#9374=DIRECTION('',(0.,0.,-1.));
#9375=DIRECTION('center_axis',(-1.,0.,0.));
#9376=DIRECTION('ref_axis',(0.,0.,1.));
#9377=DIRECTION('center_axis',(0.,-1.,0.));
#9378=DIRECTION('ref_axis',(0.,0.,-1.));
#9379=DIRECTION('center_axis',(1.,0.,0.));
#9380=DIRECTION('ref_axis',(0.,-0.707106781186548,0.707106781186547));
#9381=DIRECTION('center_axis',(-1.,0.,0.));
#9382=DIRECTION('ref_axis',(0.,-0.707106781186548,0.707106781186547));
#9383=DIRECTION('center_axis',(0.,1.,0.));
#9384=DIRECTION('ref_axis',(0.707106781186548,0.,-0.707106781186547));
#9385=DIRECTION('center_axis',(0.,-1.,0.));
#9386=DIRECTION('ref_axis',(0.,0.,-1.));
#9387=DIRECTION('',(0.,-1.,0.));
#9388=DIRECTION('',(0.,1.,0.));
#9389=DIRECTION('center_axis',(-0.816496580927725,-0.408248290463864,-0.408248290463863));
#9390=DIRECTION('ref_axis',(0.577350269189626,-0.577350269189626,-0.577350269189625));
#9391=DIRECTION('center_axis',(0.,0.,-1.));
#9392=DIRECTION('ref_axis',(0.707106781186548,-0.707106781186548,0.));
#9393=DIRECTION('center_axis',(-1.,0.,0.));
#9394=DIRECTION('ref_axis',(0.,0.707106781186547,-0.707106781186548));
#9395=DIRECTION('center_axis',(-1.,0.,0.));
#9396=DIRECTION('ref_axis',(0.,1.,1.11022302462516E-15));
#9397=DIRECTION('',(-1.,0.,0.));
#9398=DIRECTION('center_axis',(-1.,0.,0.));
#9399=DIRECTION('ref_axis',(0.,0.707106781186547,-0.707106781186548));
#9400=DIRECTION('',(1.,0.,0.));
#9401=DIRECTION('center_axis',(-0.816496580927726,0.408248290463863,-0.408248290463863));
#9402=DIRECTION('ref_axis',(0.577350269189628,0.577350269189627,-0.577350269189623));
#9403=DIRECTION('center_axis',(0.,0.,-1.));
#9404=DIRECTION('ref_axis',(0.707106781186549,0.707106781186546,0.));
#9405=DIRECTION('center_axis',(0.,-1.,0.));
#9406=DIRECTION('ref_axis',(0.,0.,-1.));
#9407=DIRECTION('',(0.,0.,1.));
#9408=DIRECTION('',(0.,0.,-1.));
#9409=DIRECTION('',(1.,0.,0.));
#9410=DIRECTION('',(0.,0.,1.));
#9411=DIRECTION('',(-1.,0.,0.));
#9412=DIRECTION('',(0.,0.,-1.));
#9413=DIRECTION('',(1.,0.,0.));
#9414=DIRECTION('',(1.,0.,0.));
#9415=DIRECTION('center_axis',(0.,0.,-1.));
#9416=DIRECTION('ref_axis',(0.707106781186548,-0.707106781186548,0.));
#9417=DIRECTION('',(0.,0.,1.));
#9418=DIRECTION('center_axis',(0.,0.,-1.));
#9419=DIRECTION('ref_axis',(1.,0.,0.));
#9420=DIRECTION('center_axis',(1.,0.,0.));
#9421=DIRECTION('ref_axis',(0.,1.,0.));
#9422=DIRECTION('',(0.,0.,-1.));
#9423=DIRECTION('',(0.,1.,0.));
#9424=DIRECTION('center_axis',(1.,0.,0.));
#9425=DIRECTION('ref_axis',(0.,-0.847202876515606,-0.531269504134844));
#9426=DIRECTION('center_axis',(1.,0.,0.));
#9427=DIRECTION('ref_axis',(0.,-0.790280212002226,-0.612745613217848));
#9428=DIRECTION('',(0.,-2.79713066068216E-16,-1.));
#9429=DIRECTION('center_axis',(-1.,0.,0.));
#9430=DIRECTION('ref_axis',(0.,0.707106781186548,0.707106781186547));
#9431=DIRECTION('',(0.,1.,0.));
#9432=DIRECTION('center_axis',(-1.,0.,0.));
#9433=DIRECTION('ref_axis',(0.,-0.707106781186549,0.707106781186546));
#9434=DIRECTION('',(0.,0.,1.));
#9435=DIRECTION('',(0.,-1.,0.));
#9436=DIRECTION('center_axis',(1.,0.,0.));
#9437=DIRECTION('ref_axis',(0.,1.,0.));
#9438=DIRECTION('',(0.,1.,0.));
#9439=DIRECTION('center_axis',(0.,0.,1.));
#9440=DIRECTION('ref_axis',(0.707106781186549,0.707106781186546,0.));
#9441=DIRECTION('',(0.,0.,1.));
#9442=DIRECTION('center_axis',(0.,0.,-1.));
#9443=DIRECTION('ref_axis',(0.,1.,0.));
#9444=DIRECTION('center_axis',(0.,1.,0.));
#9445=DIRECTION('ref_axis',(0.,0.,1.));
#9446=DIRECTION('',(0.,0.,-1.));
#9447=DIRECTION('',(1.,0.,0.));
#9448=DIRECTION('',(0.,0.,1.));
#9449=DIRECTION('',(1.,0.,0.));
#9450=DIRECTION('',(0.,0.,-1.));
#9451=DIRECTION('',(-1.,0.,0.));
#9452=DIRECTION('center_axis',(0.,1.,0.));
#9453=DIRECTION('ref_axis',(1.,0.,0.));
#9454=DIRECTION('',(-1.,0.,0.));
#9455=DIRECTION('',(0.,0.,-1.));
#9456=DIRECTION('',(1.,0.,0.));
#9457=DIRECTION('',(0.,0.,1.));
#9458=DIRECTION('center_axis',(1.,0.,0.));
#9459=DIRECTION('ref_axis',(0.,-1.,0.));
#9460=DIRECTION('',(0.,1.,0.));
#9461=DIRECTION('',(0.,0.,-1.));
#9462=DIRECTION('',(0.,-1.,0.));
#9463=DIRECTION('',(0.,0.,-1.));
#9464=DIRECTION('center_axis',(0.,0.,-1.));
#9465=DIRECTION('ref_axis',(1.,-1.11022302462516E-15,0.));
#9466=DIRECTION('center_axis',(0.,0.,1.));
#9467=DIRECTION('ref_axis',(1.,-1.11022302462516E-15,0.));
#9468=DIRECTION('center_axis',(0.,0.,-1.));
#9469=DIRECTION('ref_axis',(1.,-1.11022302462516E-15,0.));
#9470=DIRECTION('center_axis',(-1.11022302462516E-16,-1.,0.));
#9471=DIRECTION('ref_axis',(-1.,1.11022302462516E-16,0.));
#9472=DIRECTION('',(1.,-1.11022302462516E-16,0.));
#9473=DIRECTION('',(-1.,1.11022302462516E-16,0.));
#9474=DIRECTION('',(0.,0.,-1.));
#9475=DIRECTION('center_axis',(0.,0.,-1.));
#9476=DIRECTION('ref_axis',(0.,-1.,0.));
#9477=DIRECTION('center_axis',(0.,0.,1.));
#9478=DIRECTION('ref_axis',(0.,-1.,0.));
#9479=DIRECTION('center_axis',(0.,0.,-1.));
#9480=DIRECTION('ref_axis',(0.,-1.,0.));
#9481=DIRECTION('center_axis',(0.,0.,1.));
#9482=DIRECTION('ref_axis',(0.,-1.,0.));
#9483=DIRECTION('',(-1.,0.,0.));
#9484=DIRECTION('',(0.,-1.,0.));
#9485=DIRECTION('',(1.,0.,0.));
#9486=DIRECTION('',(0.,-1.,0.));
#9487=DIRECTION('center_axis',(1.,0.,0.));
#9488=DIRECTION('ref_axis',(0.,1.,0.));
#9489=DIRECTION('center_axis',(1.,0.,0.));
#9490=DIRECTION('ref_axis',(0.,1.,0.));
#9491=DIRECTION('',(0.,0.,1.));
#9492=DIRECTION('center_axis',(1.,0.,0.));
#9493=DIRECTION('ref_axis',(0.,1.,0.));
#9494=DIRECTION('',(0.,-1.,0.));
#9495=DIRECTION('center_axis',(-1.,0.,0.));
#9496=DIRECTION('ref_axis',(0.,-1.,0.));
#9497=DIRECTION('',(0.,2.79713066068216E-16,1.));
#9498=DIRECTION('',(0.,-1.,0.));
#9499=DIRECTION('center_axis',(1.,0.,0.));
#9500=DIRECTION('ref_axis',(0.,0.707106781186548,0.707106781186547));
#9501=DIRECTION('',(0.,2.79713066068216E-16,1.));
#9502=DIRECTION('center_axis',(-1.,0.,0.));
#9503=DIRECTION('ref_axis',(0.,-1.,0.));
#9504=DIRECTION('',(0.,-1.,0.));
#9505=DIRECTION('center_axis',(1.,0.,0.));
#9506=DIRECTION('ref_axis',(0.,1.,-4.44089209850062E-15));
#9507=DIRECTION('center_axis',(1.,0.,0.));
#9508=DIRECTION('ref_axis',(0.,-1.11022302462516E-15,-1.));
#9509=DIRECTION('',(0.,1.,0.));
#9510=DIRECTION('center_axis',(-1.,0.,0.));
#9511=DIRECTION('ref_axis',(0.,1.,0.));
#9512=DIRECTION('center_axis',(-1.,0.,0.));
#9513=DIRECTION('ref_axis',(0.,1.,0.));
#9514=DIRECTION('',(-1.,0.,0.));
#9515=DIRECTION('center_axis',(1.,0.,0.));
#9516=DIRECTION('ref_axis',(0.,1.,0.));
#9517=DIRECTION('',(1.,0.,0.));
#9518=DIRECTION('',(-1.,0.,0.));
#9519=DIRECTION('center_axis',(1.,0.,0.));
#9520=DIRECTION('ref_axis',(0.,1.,0.));
#9521=DIRECTION('center_axis',(-1.,0.,0.));
#9522=DIRECTION('ref_axis',(0.,1.,0.));
#9523=DIRECTION('center_axis',(-1.,0.,0.));
#9524=DIRECTION('ref_axis',(0.,1.,0.));
#9525=DIRECTION('',(-1.,0.,0.));
#9526=DIRECTION('center_axis',(1.,0.,0.));
#9527=DIRECTION('ref_axis',(0.,1.,0.));
#9528=DIRECTION('',(1.,0.,0.));
#9529=DIRECTION('center_axis',(1.,0.,0.));
#9530=DIRECTION('ref_axis',(0.,1.,0.));
#9531=DIRECTION('center_axis',(-1.,0.,0.));
#9532=DIRECTION('ref_axis',(0.,1.,0.));
#9533=DIRECTION('center_axis',(-1.,0.,0.));
#9534=DIRECTION('ref_axis',(0.,1.,0.));
#9535=DIRECTION('',(-1.,0.,0.));
#9536=DIRECTION('',(-1.,0.,0.));
#9537=DIRECTION('center_axis',(1.,0.,0.));
#9538=DIRECTION('ref_axis',(0.,1.,0.));
#9539=DIRECTION('',(1.,0.,0.));
#9540=DIRECTION('center_axis',(-1.,0.,0.));
#9541=DIRECTION('ref_axis',(0.,1.,0.));
#9542=DIRECTION('center_axis',(-1.,0.,0.));
#9543=DIRECTION('ref_axis',(0.,1.,0.));
#9544=DIRECTION('',(-1.,0.,0.));
#9545=DIRECTION('',(-1.,0.,0.));
#9546=DIRECTION('center_axis',(1.,0.,0.));
#9547=DIRECTION('ref_axis',(0.,1.,0.));
#9548=DIRECTION('center_axis',(0.,0.,1.));
#9549=DIRECTION('ref_axis',(0.,-1.,0.));
#9550=DIRECTION('',(0.,-1.,0.));
#9551=DIRECTION('',(1.,0.,0.));
#9552=DIRECTION('center_axis',(1.,0.,0.));
#9553=DIRECTION('ref_axis',(0.,1.,0.));
#9554=DIRECTION('',(0.,1.,0.));
#9555=DIRECTION('',(0.,0.,-1.));
#9556=DIRECTION('center_axis',(1.,0.,0.));
#9557=DIRECTION('ref_axis',(0.,1.,0.));
#9558=DIRECTION('',(0.,0.,1.));
#9559=DIRECTION('',(0.,1.,0.));
#9560=DIRECTION('center_axis',(-1.,0.,0.));
#9561=DIRECTION('ref_axis',(0.,0.,-1.));
#9562=DIRECTION('',(0.,-1.,0.));
#9563=DIRECTION('',(0.,0.,1.));
#9564=DIRECTION('center_axis',(0.,-1.,0.));
#9565=DIRECTION('ref_axis',(0.,0.,-1.));
#9566=DIRECTION('',(1.,0.,0.));
#9567=DIRECTION('',(0.,0.,1.));
#9568=DIRECTION('',(1.,0.,0.));
#9569=DIRECTION('center_axis',(0.,-1.,0.));
#9570=DIRECTION('ref_axis',(0.,0.,-1.));
#9571=DIRECTION('',(1.,0.,0.));
#9572=DIRECTION('',(0.,0.,1.));
#9573=DIRECTION('',(-1.,0.,0.));
#9574=DIRECTION('',(0.,0.,1.));
#9575=DIRECTION('center_axis',(0.,0.,1.));
#9576=DIRECTION('ref_axis',(0.,1.,0.));
#9577=DIRECTION('',(0.,-1.,0.));
#9578=DIRECTION('',(-1.,0.,0.));
#9579=DIRECTION('center_axis',(0.,0.,1.));
#9580=DIRECTION('ref_axis',(0.,-1.,0.));
#9581=DIRECTION('',(1.,0.,0.));
#9582=DIRECTION('',(0.,1.,0.));
#9583=DIRECTION('center_axis',(1.,0.,0.));
#9584=DIRECTION('ref_axis',(0.,1.,0.));
#9585=DIRECTION('center_axis',(1.,0.,0.));
#9586=DIRECTION('ref_axis',(0.,0.,1.));
#9587=DIRECTION('',(0.,1.,0.));
#9588=DIRECTION('',(0.,0.,-1.));
#9589=DIRECTION('',(0.,-1.,0.));
#9590=DIRECTION('',(0.,0.,1.));
#9591=DIRECTION('center_axis',(1.,0.,0.));
#9592=DIRECTION('ref_axis',(0.,1.,0.));
#9593=DIRECTION('',(0.,-1.,0.));
#9594=DIRECTION('',(0.,1.,0.));
#9595=DIRECTION('center_axis',(1.,0.,0.));
#9596=DIRECTION('ref_axis',(0.,0.,-1.));
#9597=DIRECTION('',(0.,-2.79713066068216E-16,-1.));
#9598=DIRECTION('center_axis',(1.,0.,0.));
#9599=DIRECTION('ref_axis',(0.,-1.,0.));
#9600=DIRECTION('center_axis',(0.,1.,-2.79713066068216E-16));
#9601=DIRECTION('ref_axis',(0.,2.79713066068216E-16,1.));
#9602=DIRECTION('',(1.,0.,0.));
#9603=DIRECTION('center_axis',(1.,0.,0.));
#9604=DIRECTION('ref_axis',(0.,-1.,0.));
#9605=DIRECTION('center_axis',(1.,0.,0.));
#9606=DIRECTION('ref_axis',(0.,-1.,0.));
#9607=DIRECTION('',(1.,0.,0.));
#9608=DIRECTION('center_axis',(-1.,0.,0.));
#9609=DIRECTION('ref_axis',(0.,0.,1.));
#9610=DIRECTION('center_axis',(-1.,0.,0.));
#9611=DIRECTION('ref_axis',(0.,0.,1.));
#9612=DIRECTION('',(-1.,0.,0.));
#9613=DIRECTION('center_axis',(0.,0.,-1.));
#9614=DIRECTION('ref_axis',(0.,-1.,0.));
#9615=DIRECTION('',(-1.,0.,0.));
#9616=DIRECTION('center_axis',(0.,0.,-1.));
#9617=DIRECTION('ref_axis',(0.,-1.,0.));
#9618=DIRECTION('',(0.,-1.,0.));
#9619=DIRECTION('',(1.,0.,0.));
#9620=DIRECTION('center_axis',(1.,0.,0.));
#9621=DIRECTION('ref_axis',(0.,1.,0.));
#9622=DIRECTION('',(0.,0.,-1.));
#9623=DIRECTION('center_axis',(0.,1.,0.));
#9624=DIRECTION('ref_axis',(0.,0.,1.));
#9625=DIRECTION('',(1.,0.,0.));
#9626=DIRECTION('center_axis',(-1.,0.,0.));
#9627=DIRECTION('ref_axis',(0.,0.,-1.));
#9628=DIRECTION('center_axis',(0.,0.,1.));
#9629=DIRECTION('ref_axis',(0.,1.,0.));
#9630=DIRECTION('',(-1.,0.,0.));
#9631=DIRECTION('',(0.,1.,0.));
#9632=DIRECTION('center_axis',(0.,1.,0.));
#9633=DIRECTION('ref_axis',(0.,0.,-1.));
#9634=DIRECTION('',(0.,0.,-1.));
#9635=DIRECTION('',(-1.,0.,0.));
#9636=DIRECTION('center_axis',(-1.,0.,0.));
#9637=DIRECTION('ref_axis',(0.,1.,0.));
#9638=DIRECTION('center_axis',(-1.,0.,0.));
#9639=DIRECTION('ref_axis',(0.,1.,0.));
#9640=DIRECTION('center_axis',(1.,0.,0.));
#9641=DIRECTION('ref_axis',(0.,1.,0.));
#9642=DIRECTION('center_axis',(0.,0.,1.));
#9643=DIRECTION('ref_axis',(0.,1.,0.));
#9644=DIRECTION('center_axis',(0.,1.,0.));
#9645=DIRECTION('ref_axis',(0.707106781186549,0.,-0.707106781186546));
#9646=DIRECTION('center_axis',(0.,1.,0.));
#9647=DIRECTION('ref_axis',(1.,0.,0.));
#9648=DIRECTION('',(0.,1.,0.));
#9649=DIRECTION('center_axis',(0.,-1.,0.));
#9650=DIRECTION('ref_axis',(0.,0.,-1.));
#9651=DIRECTION('center_axis',(-1.,0.,0.));
#9652=DIRECTION('ref_axis',(0.,0.,1.));
#9653=DIRECTION('center_axis',(0.,1.,0.));
#9654=DIRECTION('ref_axis',(0.,0.,1.));
#9655=DIRECTION('center_axis',(-1.,0.,0.));
#9656=DIRECTION('ref_axis',(0.,1.,0.));
#9657=DIRECTION('center_axis',(0.,-1.,0.));
#9658=DIRECTION('ref_axis',(0.707106781186549,0.,0.707106781186546));
#9659=DIRECTION('center_axis',(0.,1.,0.));
#9660=DIRECTION('ref_axis',(0.,0.,1.));
#9661=DIRECTION('',(0.,-1.,0.));
#9662=DIRECTION('center_axis',(-1.,0.,0.));
#9663=DIRECTION('ref_axis',(0.,0.,1.));
#9664=DIRECTION('center_axis',(0.,-0.96848146623447,0.249085626964569));
#9665=DIRECTION('ref_axis',(1.,0.,0.));
#9666=DIRECTION('center_axis',(-1.,0.,0.));
#9667=DIRECTION('ref_axis',(0.,-0.790280212002226,-0.612745613217848));
#9668=DIRECTION('center_axis',(0.,0.,-1.));
#9669=DIRECTION('ref_axis',(0.,1.,0.));
#9670=DIRECTION('center_axis',(0.,2.79713066068216E-16,1.));
#9671=DIRECTION('ref_axis',(0.707106781186546,0.707106781186549,0.));
#9672=DIRECTION('center_axis',(0.,0.,-1.));
#9673=DIRECTION('ref_axis',(0.,1.,0.));
#9674=DIRECTION('',(0.,2.79713066068216E-16,1.));
#9675=DIRECTION('center_axis',(0.,1.,0.));
#9676=DIRECTION('ref_axis',(0.,0.,1.));
#9677=DIRECTION('center_axis',(1.,0.,0.));
#9678=DIRECTION('ref_axis',(0.,0.707106781186548,0.707106781186547));
#9679=DIRECTION('center_axis',(0.,-1.,0.));
#9680=DIRECTION('ref_axis',(0.707106781186549,0.,0.707106781186546));
#9681=DIRECTION('center_axis',(0.,1.,0.));
#9682=DIRECTION('ref_axis',(0.,0.,1.));
#9683=DIRECTION('center_axis',(0.,0.,1.));
#9684=DIRECTION('ref_axis',(0.,-1.,0.));
#9685=DIRECTION('center_axis',(1.,0.,0.));
#9686=DIRECTION('ref_axis',(0.,-0.707106781186549,0.707106781186546));
#9687=DIRECTION('center_axis',(0.,0.,-1.));
#9688=DIRECTION('ref_axis',(0.707106781186548,-0.707106781186548,0.));
#9689=DIRECTION('center_axis',(0.,0.,1.));
#9690=DIRECTION('ref_axis',(0.,-1.,0.));
#9691=DIRECTION('center_axis',(0.,-1.,0.));
#9692=DIRECTION('ref_axis',(0.707106781186549,0.,0.707106781186546));
#9693=DIRECTION('center_axis',(0.,-1.,0.));
#9694=DIRECTION('ref_axis',(1.,0.,0.));
#9695=DIRECTION('',(0.,-1.,0.));
#9696=DIRECTION('center_axis',(0.,1.,0.));
#9697=DIRECTION('ref_axis',(0.,0.,1.));
#9698=DIRECTION('center_axis',(-1.,0.,0.));
#9699=DIRECTION('ref_axis',(0.,0.,1.));
#9700=DIRECTION('center_axis',(0.,-0.435505427952634,-0.900186104216119));
#9701=DIRECTION('ref_axis',(0.,0.900186104216119,-0.435505427952634));
#9702=DIRECTION('center_axis',(-1.,0.,0.));
#9703=DIRECTION('ref_axis',(0.,-0.847202876515606,-0.531269504134844));
#9704=DIRECTION('center_axis',(-0.816496580927726,0.408248290463863,0.408248290463863));
#9705=DIRECTION('ref_axis',(0.577350269189628,0.577350269189627,0.577350269189623));
#9706=DIRECTION('center_axis',(1.,0.,0.));
#9707=DIRECTION('ref_axis',(0.,0.707106781186548,0.707106781186548));
#9708=DIRECTION('center_axis',(0.,0.,1.));
#9709=DIRECTION('ref_axis',(1.,0.,0.));
#9710=DIRECTION('center_axis',(1.,0.,0.));
#9711=DIRECTION('ref_axis',(0.,-0.249085626964568,-0.96848146623447));
#9712=DIRECTION('center_axis',(-0.816496580927726,-0.408248290463865,-0.40824829046386));
#9713=DIRECTION('ref_axis',(0.577350269189627,-0.577350269189627,-0.577350269189623));
#9714=DIRECTION('center_axis',(1.,0.,0.));
#9715=DIRECTION('ref_axis',(0.,-0.707106781186549,-0.707106781186546));
#9716=DIRECTION('center_axis',(-0.816496580927725,-0.408248290463865,0.408248290463863));
#9717=DIRECTION('ref_axis',(0.577350269189627,-0.577350269189627,0.577350269189623));
#9718=DIRECTION('center_axis',(1.,0.,0.));
#9719=DIRECTION('ref_axis',(0.,-0.707106781186549,0.707106781186546));
#9720=DIRECTION('center_axis',(-1.,0.,0.));
#9721=DIRECTION('ref_axis',(0.,-0.707106781186549,0.707106781186546));
#9722=DIRECTION('',(-1.,0.,0.));
#9723=DIRECTION('center_axis',(-1.,0.,0.));
#9724=DIRECTION('ref_axis',(0.,-0.707106781186549,0.707106781186546));
#9725=DIRECTION('center_axis',(0.,0.,-1.));
#9726=DIRECTION('ref_axis',(0.,-1.,0.));
#9727=DIRECTION('',(-1.,0.,0.));
#9728=DIRECTION('',(0.,-1.,0.));
#9729=DIRECTION('center_axis',(-1.,0.,0.));
#9730=DIRECTION('ref_axis',(0.,0.,-1.));
#9731=DIRECTION('',(-1.,0.,0.));
#9732=DIRECTION('center_axis',(-1.,0.,0.));
#9733=DIRECTION('ref_axis',(0.,0.,-1.));
#9734=DIRECTION('center_axis',(0.,0.,1.));
#9735=DIRECTION('ref_axis',(0.,1.,0.));
#9736=DIRECTION('',(1.,0.,0.));
#9737=DIRECTION('',(0.,1.,0.));
#9738=DIRECTION('center_axis',(1.,0.,0.));
#9739=DIRECTION('ref_axis',(0.,-0.707106781186549,-0.707106781186546));
#9740=DIRECTION('center_axis',(-1.,0.,0.));
#9741=DIRECTION('ref_axis',(0.,-0.707106781186549,-0.707106781186546));
#9742=DIRECTION('center_axis',(1.,0.,0.));
#9743=DIRECTION('ref_axis',(0.,-0.707106781186549,0.707106781186546));
#9744=DIRECTION('center_axis',(1.,0.,0.));
#9745=DIRECTION('ref_axis',(0.,0.707106781186548,0.707106781186547));
#9746=DIRECTION('',(-1.,0.,0.));
#9747=DIRECTION('center_axis',(0.,1.,-2.79713066068216E-16));
#9748=DIRECTION('ref_axis',(0.,2.79713066068216E-16,1.));
#9749=DIRECTION('',(1.,0.,0.));
#9750=DIRECTION('center_axis',(1.,0.,0.));
#9751=DIRECTION('ref_axis',(0.,-1.,0.));
#9752=DIRECTION('',(1.,0.,0.));
#9753=DIRECTION('center_axis',(-1.,0.,0.));
#9754=DIRECTION('ref_axis',(0.,-1.,0.));
#9755=DIRECTION('',(1.,0.,0.));
#9756=DIRECTION('center_axis',(-1.,0.,0.));
#9757=DIRECTION('ref_axis',(0.,-0.249085626964568,-0.96848146623447));
#9758=DIRECTION('',(-1.,0.,0.));
#9759=DIRECTION('center_axis',(-1.,0.,0.));
#9760=DIRECTION('ref_axis',(0.,-0.249085626964568,-0.96848146623447));
#9761=DIRECTION('center_axis',(-1.,0.,0.));
#9762=DIRECTION('ref_axis',(0.,0.,1.));
#9763=DIRECTION('',(-1.,0.,0.));
#9764=DIRECTION('center_axis',(-1.,0.,0.));
#9765=DIRECTION('ref_axis',(0.,0.,1.));
#9766=DIRECTION('center_axis',(0.,0.,-1.));
#9767=DIRECTION('ref_axis',(0.,-1.,0.));
#9768=DIRECTION('',(1.,0.,0.));
#9769=DIRECTION('',(0.,-1.,0.));
#9770=DIRECTION('center_axis',(1.,0.,0.));
#9771=DIRECTION('ref_axis',(0.,0.707106781186548,0.707106781186548));
#9772=DIRECTION('center_axis',(-1.,0.,0.));
#9773=DIRECTION('ref_axis',(0.,0.707106781186548,0.707106781186548));
#9774=DIRECTION('center_axis',(0.,0.,1.));
#9775=DIRECTION('ref_axis',(0.,1.,0.));
#9776=DIRECTION('',(0.,1.,0.));
#9777=DIRECTION('',(-1.,0.,0.));
#9778=DIRECTION('center_axis',(0.,1.,0.));
#9779=DIRECTION('ref_axis',(0.,0.,-1.));
#9780=DIRECTION('',(-1.,0.,0.));
#9781=DIRECTION('',(0.,0.,-1.));
#9782=DIRECTION('',(-1.,0.,0.));
#9783=DIRECTION('center_axis',(-1.,0.,0.));
#9784=DIRECTION('ref_axis',(0.,1.,0.));
#9785=DIRECTION('center_axis',(-1.,0.,0.));
#9786=DIRECTION('ref_axis',(0.,1.,0.));
#9787=DIRECTION('center_axis',(1.,0.,0.));
#9788=DIRECTION('ref_axis',(0.,1.,0.));
#9789=DIRECTION('center_axis',(-1.,0.,0.));
#9790=DIRECTION('ref_axis',(0.,-1.,0.));
#9791=DIRECTION('',(0.,-1.,0.));
#9792=DIRECTION('center_axis',(1.,0.,0.));
#9793=DIRECTION('ref_axis',(0.,1.,0.));
#9794=DIRECTION('',(0.,-1.,0.));
#9795=DIRECTION('center_axis',(-1.,0.,0.));
#9796=DIRECTION('ref_axis',(0.,1.,-4.44089209850062E-15));
#9797=DIRECTION('center_axis',(0.,0.,1.));
#9798=DIRECTION('ref_axis',(0.,1.,0.));
#9799=DIRECTION('',(-1.,0.,0.));
#9800=DIRECTION('',(0.,1.,0.));
#9801=DIRECTION('center_axis',(-1.,0.,0.));
#9802=DIRECTION('ref_axis',(0.,0.,1.));
#9803=DIRECTION('',(-1.,0.,0.));
#9804=DIRECTION('center_axis',(-1.,0.,0.));
#9805=DIRECTION('ref_axis',(0.,0.,1.));
#9806=DIRECTION('center_axis',(0.,-1.,0.));
#9807=DIRECTION('ref_axis',(0.,0.,1.));
#9808=DIRECTION('',(1.,0.,0.));
#9809=DIRECTION('',(0.,0.,1.));
#9810=DIRECTION('center_axis',(1.,0.,0.));
#9811=DIRECTION('ref_axis',(0.,1.,0.));
#9812=DIRECTION('',(0.,-1.,0.));
#9813=DIRECTION('center_axis',(-1.,0.,0.));
#9814=DIRECTION('ref_axis',(0.,-1.11022302462516E-15,-1.));
#9815=DIRECTION('center_axis',(1.,0.,0.));
#9816=DIRECTION('ref_axis',(0.,1.,0.));
#9817=DIRECTION('center_axis',(0.,0.,1.));
#9818=DIRECTION('ref_axis',(0.,-1.,0.));
#9819=DIRECTION('',(1.,0.,0.));
#9820=DIRECTION('center_axis',(0.,0.,-1.));
#9821=DIRECTION('ref_axis',(0.,1.,0.));
#9822=DIRECTION('',(1.,0.,0.));
#9823=DIRECTION('',(1.,0.,0.));
#9824=DIRECTION('center_axis',(1.,0.,0.));
#9825=DIRECTION('ref_axis',(0.,1.,-4.44089209850062E-15));
#9826=DIRECTION('center_axis',(1.,0.,0.));
#9827=DIRECTION('ref_axis',(0.,-1.11022302462516E-15,-1.));
#9828=DIRECTION('center_axis',(1.,0.,0.));
#9829=DIRECTION('ref_axis',(0.,-1.,0.));
#9830=DIRECTION('axis',(0.,0.,1.));
#9831=DIRECTION('refdir',(1.,0.,0.));
#9832=DIRECTION('center_axis',(-1.,0.,0.));
#9833=DIRECTION('ref_axis',(0.,-1.,0.));
#9834=DIRECTION('',(0.,0.,-1.));
#9835=DIRECTION('',(0.,-1.,-3.48381790312471E-17));
#9836=DIRECTION('center_axis',(-1.,0.,0.));
#9837=DIRECTION('ref_axis',(0.,1.,1.66533453693774E-15));
#9838=DIRECTION('',(0.,8.3698837981778E-17,-1.));
#9839=DIRECTION('center_axis',(-1.,0.,0.));
#9840=DIRECTION('ref_axis',(0.,-1.11022302462516E-15,1.));
#9841=DIRECTION('',(0.,1.,0.));
#9842=DIRECTION('center_axis',(-1.,0.,0.));
#9843=DIRECTION('ref_axis',(0.,6.66133814775096E-15,-1.));
#9844=DIRECTION('',(0.,-8.00068553810663E-16,-1.));
#9845=DIRECTION('center_axis',(-1.,0.,0.));
#9846=DIRECTION('ref_axis',(0.,2.2204460492503E-15,1.));
#9847=DIRECTION('',(0.,1.,0.));
#9848=DIRECTION('',(0.,0.,-1.));
#9849=DIRECTION('',(0.,1.,0.));
#9850=DIRECTION('',(0.,-8.00068553810663E-16,-1.));
#9851=DIRECTION('center_axis',(1.,0.,0.));
#9852=DIRECTION('ref_axis',(0.,6.66133814775096E-15,-1.));
#9853=DIRECTION('center_axis',(1.,0.,0.));
#9854=DIRECTION('ref_axis',(0.,1.,0.));
#9855=DIRECTION('',(0.,8.3698837981778E-17,-1.));
#9856=DIRECTION('center_axis',(1.,0.,0.));
#9857=DIRECTION('ref_axis',(0.,1.,0.));
#9858=DIRECTION('center_axis',(-1.,0.,0.));
#9859=DIRECTION('ref_axis',(0.,1.,0.));
#9860=DIRECTION('center_axis',(-1.,0.,0.));
#9861=DIRECTION('ref_axis',(0.,1.,0.));
#9862=DIRECTION('center_axis',(-1.,0.,0.));
#9863=DIRECTION('ref_axis',(0.,0.,-1.));
#9864=DIRECTION('center_axis',(0.,0.,-1.));
#9865=DIRECTION('ref_axis',(-0.258819045102521,-0.965925826289068,0.));
#9866=DIRECTION('center_axis',(1.11022302462516E-15,-1.,0.));
#9867=DIRECTION('ref_axis',(-1.,-1.11022302462516E-15,0.));
#9868=DIRECTION('center_axis',(0.,0.,1.));
#9869=DIRECTION('ref_axis',(-0.258819045102521,-0.965925826289068,0.));
#9870=DIRECTION('center_axis',(-1.,0.,0.));
#9871=DIRECTION('ref_axis',(0.,-0.707106781186547,-0.707106781186548));
#9872=DIRECTION('center_axis',(-1.,0.,0.));
#9873=DIRECTION('ref_axis',(0.,0.,-1.));
#9874=DIRECTION('',(-1.,0.,0.));
#9875=DIRECTION('',(1.,0.,0.));
#9876=DIRECTION('center_axis',(3.33066907387547E-15,1.,-3.69778549322349E-30));
#9877=DIRECTION('ref_axis',(-1.11022302462516E-15,0.,-1.));
#9878=DIRECTION('center_axis',(0.,0.,-1.));
#9879=DIRECTION('ref_axis',(-0.258819045102521,0.965925826289068,0.));
#9880=DIRECTION('center_axis',(-1.,0.,0.));
#9881=DIRECTION('ref_axis',(0.,1.,0.));
#9882=DIRECTION('center_axis',(0.,0.,1.));
#9883=DIRECTION('ref_axis',(-0.258819045102521,0.965925826289068,0.));
#9884=DIRECTION('center_axis',(1.,0.,0.));
#9885=DIRECTION('ref_axis',(0.,0.707106781186547,-0.707106781186548));
#9886=DIRECTION('',(-1.,0.,0.));
#9887=DIRECTION('',(1.,0.,0.));
#9888=DIRECTION('center_axis',(-0.707106781186547,0.707106781186548,-7.85046229341886E-16));
#9889=DIRECTION('ref_axis',(-0.707106781186548,-0.707106781186547,7.85046229341885E-16));
#9890=DIRECTION('center_axis',(0.,-1.,0.));
#9891=DIRECTION('ref_axis',(0.707106781186547,0.,-0.707106781186548));
#9892=DIRECTION('',(0.,-1.,0.));
#9893=DIRECTION('center_axis',(0.,1.,0.));
#9894=DIRECTION('ref_axis',(1.,0.,0.));
#9895=DIRECTION('',(0.,1.,0.));
#9896=DIRECTION('center_axis',(0.,0.,-1.));
#9897=DIRECTION('ref_axis',(0.707106781186548,-0.707106781186548,0.));
#9898=DIRECTION('center_axis',(0.,0.,1.));
#9899=DIRECTION('ref_axis',(0.707106781186547,-0.707106781186547,0.));
#9900=DIRECTION('center_axis',(0.,0.,-1.));
#9901=DIRECTION('ref_axis',(0.,-1.,0.));
#9902=DIRECTION('',(0.,0.,-1.));
#9903=DIRECTION('center_axis',(0.,-3.48381790312471E-17,1.));
#9904=DIRECTION('ref_axis',(0.,-1.,0.));
#9905=DIRECTION('',(0.,0.,-1.));
#9906=DIRECTION('center_axis',(0.,-1.,0.));
#9907=DIRECTION('ref_axis',(-1.,0.,0.));
#9908=DIRECTION('',(0.,0.,-1.));
#9909=DIRECTION('',(1.,0.,0.));
#9910=DIRECTION('center_axis',(0.,0.,-1.));
#9911=DIRECTION('ref_axis',(0.707106781186548,-0.707106781186548,0.));
#9912=DIRECTION('',(0.,0.,1.));
#9913=DIRECTION('',(0.,-1.,-3.48381790312471E-17));
#9914=DIRECTION('center_axis',(0.,-3.48381790312471E-17,1.));
#9915=DIRECTION('ref_axis',(0.707106781186548,-0.707106781186548,0.));
#9916=DIRECTION('center_axis',(1.,0.,0.));
#9917=DIRECTION('ref_axis',(0.,-1.,0.));
#9918=DIRECTION('',(0.,0.,-1.));
#9919=DIRECTION('',(0.,-1.,-3.48381790312471E-17));
#9920=DIRECTION('center_axis',(1.,0.,0.));
#9921=DIRECTION('ref_axis',(0.,-1.,0.));
#9922=DIRECTION('center_axis',(0.,-1.,0.));
#9923=DIRECTION('ref_axis',(1.,0.,0.));
#9924=DIRECTION('',(0.,0.,-1.));
#9925=DIRECTION('',(1.,0.,0.));
#9926=DIRECTION('',(0.,0.,1.));
#9927=DIRECTION('',(-1.,0.,0.));
#9928=DIRECTION('',(0.,0.,1.));
#9929=DIRECTION('center_axis',(0.,1.,0.));
#9930=DIRECTION('ref_axis',(-0.707106781186548,0.,-0.707106781186548));
#9931=DIRECTION('',(0.,1.,0.));
#9932=DIRECTION('',(0.,-1.,0.));
#9933=DIRECTION('center_axis',(0.,0.,-1.));
#9934=DIRECTION('ref_axis',(-1.,1.66533453693773E-15,0.));
#9935=DIRECTION('',(0.,0.,-1.));
#9936=DIRECTION('center_axis',(0.,-3.48381790312471E-17,1.));
#9937=DIRECTION('ref_axis',(-1.,1.66533453693773E-15,0.));
#9938=DIRECTION('center_axis',(0.,0.,-1.));
#9939=DIRECTION('ref_axis',(1.,0.,0.));
#9940=DIRECTION('center_axis',(0.,3.48381790312471E-17,-1.));
#9941=DIRECTION('ref_axis',(0.,-1.,-3.48381790312471E-17));
#9942=DIRECTION('',(0.,-1.,-3.48381790312471E-17));
#9943=DIRECTION('',(-1.,0.,0.));
#9944=DIRECTION('',(0.,-1.,-3.48381790312471E-17));
#9945=DIRECTION('',(-1.,0.,0.));
#9946=DIRECTION('',(-1.,0.,0.));
#9947=DIRECTION('center_axis',(0.,-3.48381790312471E-17,1.));
#9948=DIRECTION('ref_axis',(-1.,0.,0.));
#9949=DIRECTION('',(0.,-1.,-3.48381790312471E-17));
#9950=DIRECTION('center_axis',(0.,-3.48381790312471E-17,1.));
#9951=DIRECTION('ref_axis',(2.22044604925031E-15,-1.,0.));
#9952=DIRECTION('',(0.,-1.,-3.48381790312471E-17));
#9953=DIRECTION('center_axis',(1.,0.,0.));
#9954=DIRECTION('ref_axis',(0.,-1.,0.));
#9955=DIRECTION('center_axis',(1.,0.,0.));
#9956=DIRECTION('ref_axis',(0.,-1.,0.));
#9957=DIRECTION('',(1.,0.,0.));
#9958=DIRECTION('center_axis',(-1.,0.,0.));
#9959=DIRECTION('ref_axis',(0.,1.,0.));
#9960=DIRECTION('center_axis',(0.,1.,0.));
#9961=DIRECTION('ref_axis',(-1.,0.,0.));
#9962=DIRECTION('',(1.,0.,0.));
#9963=DIRECTION('',(0.,0.,1.));
#9964=DIRECTION('center_axis',(-1.,0.,0.));
#9965=DIRECTION('ref_axis',(0.,-1.,0.));
#9966=DIRECTION('',(0.,0.,1.));
#9967=DIRECTION('',(0.,1.,3.48381790312471E-17));
#9968=DIRECTION('',(0.,0.,1.));
#9969=DIRECTION('center_axis',(0.,0.,1.));
#9970=DIRECTION('ref_axis',(-1.,0.,0.));
#9971=DIRECTION('center_axis',(0.,3.48381790312471E-17,-1.));
#9972=DIRECTION('ref_axis',(-1.,0.,0.));
#9973=DIRECTION('center_axis',(0.,0.,1.));
#9974=DIRECTION('ref_axis',(2.22044604925031E-15,-1.,0.));
#9975=DIRECTION('center_axis',(0.,3.48381790312471E-17,-1.));
#9976=DIRECTION('ref_axis',(2.22044604925031E-15,-1.,0.));
#9977=DIRECTION('center_axis',(-1.,0.,0.));
#9978=DIRECTION('ref_axis',(0.,-1.,0.));
#9979=DIRECTION('',(0.,-1.,-3.48381790312471E-17));
#9980=DIRECTION('center_axis',(1.,0.,0.));
#9981=DIRECTION('ref_axis',(0.,1.,0.));
#9982=DIRECTION('',(0.,-3.17503269079253E-17,1.));
#9983=DIRECTION('center_axis',(1.,0.,0.));
#9984=DIRECTION('ref_axis',(0.,1.,0.));
#9985=DIRECTION('',(0.,-3.17503269079253E-17,1.));
#9986=DIRECTION('',(0.,1.,0.));
#9987=DIRECTION('',(0.,0.,1.));
#9988=DIRECTION('',(0.,1.,0.));
#9989=DIRECTION('center_axis',(-1.,0.,0.));
#9990=DIRECTION('ref_axis',(0.,-1.,0.));
#9991=DIRECTION('',(0.,-3.17503269079253E-17,1.));
#9992=DIRECTION('center_axis',(-1.,0.,0.));
#9993=DIRECTION('ref_axis',(0.,2.22044604925032E-15,-1.));
#9994=DIRECTION('center_axis',(-1.,0.,0.));
#9995=DIRECTION('ref_axis',(0.,1.,0.));
#9996=DIRECTION('center_axis',(-1.,0.,0.));
#9997=DIRECTION('ref_axis',(0.,1.,0.));
#9998=DIRECTION('center_axis',(0.,0.,-1.));
#9999=DIRECTION('ref_axis',(-1.,1.11022302462516E-15,0.));
#10000=DIRECTION('center_axis',(0.,0.,1.));
#10001=DIRECTION('ref_axis',(-1.,1.11022302462516E-15,0.));
#10002=DIRECTION('',(0.,0.,-1.));
#10003=DIRECTION('center_axis',(0.,0.,-1.));
#10004=DIRECTION('ref_axis',(-1.,1.11022302462516E-15,0.));
#10005=DIRECTION('',(0.,0.,-1.));
#10006=DIRECTION('center_axis',(-1.11022302462516E-16,-1.,0.));
#10007=DIRECTION('ref_axis',(-1.,1.11022302462516E-16,0.));
#10008=DIRECTION('',(1.,-1.11022302462516E-16,0.));
#10009=DIRECTION('',(-1.,1.11022302462516E-16,0.));
#10010=DIRECTION('center_axis',(0.,1.,0.));
#10011=DIRECTION('ref_axis',(1.,0.,0.));
#10012=DIRECTION('',(-1.,0.,0.));
#10013=DIRECTION('',(1.,0.,0.));
#10014=DIRECTION('',(0.,0.,-1.));
#10015=DIRECTION('center_axis',(0.,0.,-1.));
#10016=DIRECTION('ref_axis',(1.11022302462516E-15,1.,0.));
#10017=DIRECTION('center_axis',(0.,0.,1.));
#10018=DIRECTION('ref_axis',(1.11022302462516E-15,1.,0.));
#10019=DIRECTION('center_axis',(0.,0.,-1.));
#10020=DIRECTION('ref_axis',(1.11022302462516E-15,1.,0.));
#10021=DIRECTION('',(0.,0.,-1.));
#10022=DIRECTION('center_axis',(-1.,0.,0.));
#10023=DIRECTION('ref_axis',(0.,1.,0.));
#10024=DIRECTION('',(0.,-1.,0.));
#10025=DIRECTION('',(0.,1.,0.));
#10026=DIRECTION('center_axis',(0.,0.,1.));
#10027=DIRECTION('ref_axis',(0.,1.,0.));
#10028=DIRECTION('',(-1.,0.,0.));
#10029=DIRECTION('',(0.,1.,0.));
#10030=DIRECTION('',(-1.,0.,0.));
#10031=DIRECTION('center_axis',(0.,3.48381790312471E-17,-1.));
#10032=DIRECTION('ref_axis',(0.,-1.,-3.48381790312471E-17));
#10033=DIRECTION('',(-1.,0.,0.));
#10034=DIRECTION('',(0.,-1.,-3.48381790312471E-17));
#10035=DIRECTION('',(1.,0.,0.));
#10036=DIRECTION('center_axis',(-1.,0.,0.));
#10037=DIRECTION('ref_axis',(0.,-1.,0.));
#10038=DIRECTION('center_axis',(-1.,0.,0.));
#10039=DIRECTION('ref_axis',(0.,1.,0.));
#10040=DIRECTION('',(0.,-8.3698837981778E-17,1.));
#10041=DIRECTION('center_axis',(-1.,0.,0.));
#10042=DIRECTION('ref_axis',(0.,1.,0.));
#10043=DIRECTION('center_axis',(-1.,0.,0.));
#10044=DIRECTION('ref_axis',(0.,6.66133814775096E-15,-1.));
#10045=DIRECTION('',(0.,8.00068553810663E-16,1.));
#10046=DIRECTION('',(0.,1.,0.));
#10047=DIRECTION('',(0.,-3.17503269079253E-17,1.));
#10048=DIRECTION('center_axis',(-1.,0.,0.));
#10049=DIRECTION('ref_axis',(0.,1.,0.));
#10050=DIRECTION('',(0.,-3.17503269079253E-17,1.));
#10051=DIRECTION('center_axis',(-1.,0.,0.));
#10052=DIRECTION('ref_axis',(0.,1.,0.));
#10053=DIRECTION('center_axis',(0.,1.,8.3698837981778E-17));
#10054=DIRECTION('ref_axis',(0.,8.3698837981778E-17,-1.));
#10055=DIRECTION('',(1.,0.,0.));
#10056=DIRECTION('',(-1.,0.,0.));
#10057=DIRECTION('center_axis',(0.,-1.,-3.17503269079253E-17));
#10058=DIRECTION('ref_axis',(0.,-3.17503269079253E-17,1.));
#10059=DIRECTION('',(-1.,0.,0.));
#10060=DIRECTION('',(1.,0.,0.));
#10061=DIRECTION('center_axis',(0.,-1.,-3.17503269079253E-17));
#10062=DIRECTION('ref_axis',(0.,-3.17503269079253E-17,1.));
#10063=DIRECTION('',(1.,0.,0.));
#10064=DIRECTION('',(-1.,0.,0.));
#10065=DIRECTION('center_axis',(-1.,0.,0.));
#10066=DIRECTION('ref_axis',(0.,6.66133814775096E-15,-1.));
#10067=DIRECTION('',(1.,0.,0.));
#10068=DIRECTION('',(-1.,0.,0.));
#10069=DIRECTION('center_axis',(0.,0.,1.));
#10070=DIRECTION('ref_axis',(0.,1.,0.));
#10071=DIRECTION('',(1.,0.,0.));
#10072=DIRECTION('center_axis',(-1.,0.,0.));
#10073=DIRECTION('ref_axis',(0.,-0.715401949147516,-0.69871313938979));
#10074=DIRECTION('center_axis',(-1.,0.,0.));
#10075=DIRECTION('ref_axis',(0.,1.,0.));
#10076=DIRECTION('center_axis',(-1.,0.,0.));
#10077=DIRECTION('ref_axis',(0.,1.,0.));
#10078=DIRECTION('center_axis',(-1.,0.,0.));
#10079=DIRECTION('ref_axis',(0.,-0.728392179415956,0.685160443228937));
#10080=DIRECTION('center_axis',(0.,1.,-8.00068553810663E-16));
#10081=DIRECTION('ref_axis',(0.,-8.00068553810663E-16,-1.));
#10082=DIRECTION('center_axis',(-1.,0.,0.));
#10083=DIRECTION('ref_axis',(0.,1.,0.));
#10084=DIRECTION('',(-1.,0.,0.));
#10085=DIRECTION('center_axis',(-1.,0.,0.));
#10086=DIRECTION('ref_axis',(0.,1.,0.));
#10087=DIRECTION('center_axis',(1.,0.,0.));
#10088=DIRECTION('ref_axis',(0.,1.,0.));
#10089=DIRECTION('center_axis',(-1.,0.,0.));
#10090=DIRECTION('ref_axis',(0.,1.,0.));
#10091=DIRECTION('',(-1.,0.,0.));
#10092=DIRECTION('center_axis',(-1.,0.,0.));
#10093=DIRECTION('ref_axis',(0.,1.,0.));
#10094=DIRECTION('center_axis',(1.,0.,0.));
#10095=DIRECTION('ref_axis',(0.,1.,0.));
#10096=DIRECTION('center_axis',(-1.,0.,0.));
#10097=DIRECTION('ref_axis',(0.,1.,0.));
#10098=DIRECTION('',(-1.,0.,0.));
#10099=DIRECTION('center_axis',(-1.,0.,0.));
#10100=DIRECTION('ref_axis',(0.,1.,0.));
#10101=DIRECTION('center_axis',(1.,0.,0.));
#10102=DIRECTION('ref_axis',(0.,1.,0.));
#10103=DIRECTION('center_axis',(-1.,0.,0.));
#10104=DIRECTION('ref_axis',(0.,1.,0.));
#10105=DIRECTION('',(-1.,0.,0.));
#10106=DIRECTION('center_axis',(-1.,0.,0.));
#10107=DIRECTION('ref_axis',(0.,1.,0.));
#10108=DIRECTION('center_axis',(1.,0.,0.));
#10109=DIRECTION('ref_axis',(0.,1.,0.));
#10110=DIRECTION('center_axis',(0.,-8.00068553810663E-16,-1.));
#10111=DIRECTION('ref_axis',(-0.707106781186546,0.707106781186549,0.));
#10112=DIRECTION('center_axis',(0.,0.,-1.));
#10113=DIRECTION('ref_axis',(-1.,0.,0.));
#10114=DIRECTION('',(0.,-8.00068553810663E-16,-1.));
#10115=DIRECTION('center_axis',(0.,0.,1.));
#10116=DIRECTION('ref_axis',(0.,1.,0.));
#10117=DIRECTION('',(0.,8.00068553810663E-16,1.));
#10118=DIRECTION('center_axis',(1.,0.,0.));
#10119=DIRECTION('ref_axis',(0.,0.,-1.));
#10120=DIRECTION('center_axis',(0.,-1.,-6.66133814775096E-15));
#10121=DIRECTION('ref_axis',(0.,-6.66133814775096E-15,1.));
#10122=DIRECTION('center_axis',(-1.,0.,0.));
#10123=DIRECTION('ref_axis',(0.,-0.707106781186542,-0.707106781186553));
#10124=DIRECTION('center_axis',(1.,0.,0.));
#10125=DIRECTION('ref_axis',(0.,-0.707106781186542,-0.707106781186553));
#10126=DIRECTION('center_axis',(0.,1.,0.));
#10127=DIRECTION('ref_axis',(-0.707106781186549,0.,0.707106781186546));
#10128=DIRECTION('center_axis',(0.,-1.,0.));
#10129=DIRECTION('ref_axis',(0.,0.,1.));
#10130=DIRECTION('',(0.,-1.,0.));
#10131=DIRECTION('',(0.,1.,0.));
#10132=DIRECTION('center_axis',(0.,8.88178419700124E-15,1.));
#10133=DIRECTION('ref_axis',(0.,1.,-8.88178419700124E-15));
#10134=DIRECTION('center_axis',(1.,0.,0.));
#10135=DIRECTION('ref_axis',(0.,0.707106781186551,0.707106781186544));
#10136=DIRECTION('center_axis',(-1.,0.,0.));
#10137=DIRECTION('ref_axis',(0.,0.707106781186551,0.707106781186544));
#10138=DIRECTION('center_axis',(0.,8.3698837981778E-17,-1.));
#10139=DIRECTION('ref_axis',(-0.707106781186546,0.707106781186549,0.));
#10140=DIRECTION('center_axis',(0.,0.,1.));
#10141=DIRECTION('ref_axis',(0.,1.,0.));
#10142=DIRECTION('',(0.,-8.3698837981778E-17,1.));
#10143=DIRECTION('',(0.,8.3698837981778E-17,-1.));
#10144=DIRECTION('center_axis',(0.,1.,-2.22044604925031E-15));
#10145=DIRECTION('ref_axis',(0.,-2.22044604925031E-15,-1.));
#10146=DIRECTION('center_axis',(1.,0.,0.));
#10147=DIRECTION('ref_axis',(0.,0.707106781186549,-0.707106781186547));
#10148=DIRECTION('center_axis',(-1.,0.,0.));
#10149=DIRECTION('ref_axis',(0.,0.707106781186548,-0.707106781186547));
#10150=DIRECTION('center_axis',(0.,-1.,-3.48381790312471E-17));
#10151=DIRECTION('ref_axis',(-0.707106781186548,0.,-0.707106781186547));
#10152=DIRECTION('center_axis',(0.,1.,2.22044604925031E-15));
#10153=DIRECTION('ref_axis',(0.,2.22044604925031E-15,-1.));
#10154=DIRECTION('',(0.,1.,3.48381790312471E-17));
#10155=DIRECTION('center_axis',(0.,-8.32667268468869E-16,-1.));
#10156=DIRECTION('ref_axis',(0.,-1.,8.32667268468868E-16));
#10157=DIRECTION('center_axis',(1.,0.,0.));
#10158=DIRECTION('ref_axis',(0.,-0.707106781186547,-0.707106781186548));
#10159=DIRECTION('center_axis',(-1.,0.,0.));
#10160=DIRECTION('ref_axis',(0.,-0.707106781186547,-0.707106781186548));
#10161=DIRECTION('center_axis',(0.,-3.17503269079253E-17,1.));
#10162=DIRECTION('ref_axis',(-0.707106781186549,-0.707106781186546,0.));
#10163=DIRECTION('center_axis',(0.,0.,-1.));
#10164=DIRECTION('ref_axis',(0.,-1.,0.));
#10165=DIRECTION('',(0.,3.17503269079253E-17,-1.));
#10166=DIRECTION('',(0.,-3.17503269079253E-17,1.));
#10167=DIRECTION('center_axis',(0.,-1.,0.));
#10168=DIRECTION('ref_axis',(0.,0.,1.));
#10169=DIRECTION('center_axis',(1.,0.,0.));
#10170=DIRECTION('ref_axis',(0.,-0.707106781186547,0.707106781186548));
#10171=DIRECTION('center_axis',(-1.,0.,0.));
#10172=DIRECTION('ref_axis',(0.,-0.707106781186547,0.707106781186548));
#10173=DIRECTION('center_axis',(0.,1.,0.));
#10174=DIRECTION('ref_axis',(-0.707106781186549,0.,0.707106781186546));
#10175=DIRECTION('center_axis',(0.,-1.,0.));
#10176=DIRECTION('ref_axis',(0.,0.,1.));
#10177=DIRECTION('',(0.,-1.,0.));
#10178=DIRECTION('center_axis',(1.,0.,0.));
#10179=DIRECTION('ref_axis',(0.,0.707106781186545,0.70710678118655));
#10180=DIRECTION('center_axis',(-1.,0.,0.));
#10181=DIRECTION('ref_axis',(0.,0.707106781186545,0.70710678118655));
#10182=DIRECTION('center_axis',(-1.,0.,0.));
#10183=DIRECTION('ref_axis',(0.,1.,1.66533453693774E-15));
#10184=DIRECTION('',(-1.,0.,0.));
#10185=DIRECTION('center_axis',(0.,1.,8.3698837981778E-17));
#10186=DIRECTION('ref_axis',(0.,8.3698837981778E-17,-1.));
#10187=DIRECTION('',(-1.,0.,0.));
#10188=DIRECTION('center_axis',(-1.,0.,0.));
#10189=DIRECTION('ref_axis',(0.,-1.11022302462516E-15,1.));
#10190=DIRECTION('',(-1.,0.,0.));
#10191=DIRECTION('center_axis',(0.,0.,1.));
#10192=DIRECTION('ref_axis',(0.,1.,0.));
#10193=DIRECTION('',(-1.,0.,0.));
#10194=DIRECTION('center_axis',(-1.,0.,0.));
#10195=DIRECTION('ref_axis',(0.,6.66133814775096E-15,-1.));
#10196=DIRECTION('',(-1.,0.,0.));
#10197=DIRECTION('center_axis',(0.,1.,-8.00068553810663E-16));
#10198=DIRECTION('ref_axis',(0.,-8.00068553810663E-16,-1.));
#10199=DIRECTION('',(-1.,0.,0.));
#10200=DIRECTION('center_axis',(-1.,0.,0.));
#10201=DIRECTION('ref_axis',(0.,-1.,0.));
#10202=DIRECTION('center_axis',(-1.,0.,0.));
#10203=DIRECTION('ref_axis',(0.,2.2204460492503E-15,1.));
#10204=DIRECTION('center_axis',(-1.,0.,0.));
#10205=DIRECTION('ref_axis',(0.,-1.,0.));
#10206=DIRECTION('',(-1.,0.,0.));
#10207=DIRECTION('center_axis',(0.,-1.,-3.17503269079253E-17));
#10208=DIRECTION('ref_axis',(0.,-3.17503269079253E-17,1.));
#10209=DIRECTION('',(-1.,0.,0.));
#10210=DIRECTION('center_axis',(-1.,0.,0.));
#10211=DIRECTION('ref_axis',(0.,2.22044604925032E-15,-1.));
#10212=DIRECTION('axis',(0.,0.,1.));
#10213=DIRECTION('refdir',(1.,0.,0.));
#10214=DIRECTION('center_axis',(1.,0.,0.));
#10215=DIRECTION('ref_axis',(0.,1.,0.));
#10216=DIRECTION('center_axis',(1.,0.,0.));
#10217=DIRECTION('ref_axis',(0.,1.,0.));
#10218=DIRECTION('',(1.,0.,0.));
#10219=DIRECTION('center_axis',(-1.,0.,0.));
#10220=DIRECTION('ref_axis',(0.,1.,0.));
#10221=DIRECTION('center_axis',(1.,0.,0.));
#10222=DIRECTION('ref_axis',(0.,1.,0.));
#10223=DIRECTION('center_axis',(1.,0.,0.));
#10224=DIRECTION('ref_axis',(0.,1.,0.));
#10225=DIRECTION('',(1.,0.,0.));
#10226=DIRECTION('center_axis',(-1.,0.,0.));
#10227=DIRECTION('ref_axis',(0.,1.,0.));
#10228=DIRECTION('center_axis',(1.,0.,0.));
#10229=DIRECTION('ref_axis',(0.,1.,0.));
#10230=DIRECTION('center_axis',(1.,0.,0.));
#10231=DIRECTION('ref_axis',(0.,1.,0.));
#10232=DIRECTION('',(1.,0.,0.));
#10233=DIRECTION('center_axis',(-1.,0.,0.));
#10234=DIRECTION('ref_axis',(0.,1.,0.));
#10235=DIRECTION('center_axis',(1.,0.,0.));
#10236=DIRECTION('ref_axis',(0.,1.,0.));
#10237=DIRECTION('center_axis',(1.,0.,0.));
#10238=DIRECTION('ref_axis',(0.,1.,0.));
#10239=DIRECTION('',(1.,0.,0.));
#10240=DIRECTION('center_axis',(-1.,0.,0.));
#10241=DIRECTION('ref_axis',(0.,1.,0.));
#10242=DIRECTION('center_axis',(0.,0.,1.));
#10243=DIRECTION('ref_axis',(1.,0.,0.));
#10244=DIRECTION('center_axis',(0.,0.,-1.));
#10245=DIRECTION('ref_axis',(1.11022302462516E-15,1.,0.));
#10246=DIRECTION('',(1.,0.,0.));
#10247=DIRECTION('center_axis',(0.,0.,-1.));
#10248=DIRECTION('ref_axis',(1.,-1.11022302462516E-15,0.));
#10249=DIRECTION('',(0.,-1.,0.));
#10250=DIRECTION('center_axis',(0.,0.,-1.));
#10251=DIRECTION('ref_axis',(0.,-1.,0.));
#10252=DIRECTION('',(-1.,1.38777878078145E-16,0.));
#10253=DIRECTION('center_axis',(0.,0.,-1.));
#10254=DIRECTION('ref_axis',(-1.,1.11022302462516E-15,0.));
#10255=DIRECTION('',(0.,1.,0.));
#10256=DIRECTION('center_axis',(0.,0.,1.));
#10257=DIRECTION('ref_axis',(1.,0.,0.));
#10258=DIRECTION('',(-1.,0.,0.));
#10259=DIRECTION('center_axis',(0.,0.,1.));
#10260=DIRECTION('ref_axis',(0.,1.,0.));
#10261=DIRECTION('',(0.,-1.,0.));
#10262=DIRECTION('center_axis',(0.,0.,1.));
#10263=DIRECTION('ref_axis',(-1.,0.,0.));
#10264=DIRECTION('',(1.,-1.38777878078145E-16,0.));
#10265=DIRECTION('center_axis',(0.,0.,1.));
#10266=DIRECTION('ref_axis',(0.,-1.,0.));
#10267=DIRECTION('',(0.,1.,0.));
#10268=DIRECTION('center_axis',(0.,-1.,0.));
#10269=DIRECTION('ref_axis',(1.,0.,0.));
#10270=DIRECTION('',(0.,0.,-1.));
#10271=DIRECTION('',(1.,0.,0.));
#10272=DIRECTION('',(0.,0.,1.));
#10273=DIRECTION('center_axis',(0.,0.,1.));
#10274=DIRECTION('ref_axis',(0.,1.,0.));
#10275=DIRECTION('center_axis',(0.,0.,-1.));
#10276=DIRECTION('ref_axis',(0.,1.,0.));
#10277=DIRECTION('',(0.,0.,1.));
#10278=DIRECTION('center_axis',(1.,0.,0.));
#10279=DIRECTION('ref_axis',(0.,1.,0.));
#10280=DIRECTION('',(0.,1.,0.));
#10281=DIRECTION('',(0.,0.,1.));
#10282=DIRECTION('center_axis',(0.,0.,1.));
#10283=DIRECTION('ref_axis',(-1.,0.,0.));
#10284=DIRECTION('center_axis',(0.,0.,-1.));
#10285=DIRECTION('ref_axis',(-1.,0.,0.));
#10286=DIRECTION('',(0.,0.,1.));
#10287=DIRECTION('center_axis',(1.38777878078145E-16,1.,0.));
#10288=DIRECTION('ref_axis',(-1.,1.38777878078145E-16,0.));
#10289=DIRECTION('',(-1.,1.38777878078145E-16,0.));
#10290=DIRECTION('',(0.,0.,1.));
#10291=DIRECTION('center_axis',(0.,0.,1.));
#10292=DIRECTION('ref_axis',(0.,-1.,0.));
#10293=DIRECTION('center_axis',(0.,0.,-1.));
#10294=DIRECTION('ref_axis',(0.,-1.,0.));
#10295=DIRECTION('',(0.,0.,1.));
#10296=DIRECTION('center_axis',(-1.,0.,0.));
#10297=DIRECTION('ref_axis',(0.,-1.,0.));
#10298=DIRECTION('',(0.,-1.,0.));
#10299=DIRECTION('',(0.,0.,1.));
#10300=DIRECTION('center_axis',(0.,0.,1.));
#10301=DIRECTION('ref_axis',(1.,0.,0.));
#10302=DIRECTION('center_axis',(0.,0.,-1.));
#10303=DIRECTION('ref_axis',(1.,0.,0.));
#10304=DIRECTION('center_axis',(0.,1.,0.));
#10305=DIRECTION('ref_axis',(-1.,0.,0.));
#10306=DIRECTION('',(0.,0.,-1.));
#10307=DIRECTION('',(-1.,0.,0.));
#10308=DIRECTION('',(0.,0.,1.));
#10309=DIRECTION('center_axis',(0.,0.,1.));
#10310=DIRECTION('ref_axis',(1.,-1.11022302462516E-15,0.));
#10311=DIRECTION('center_axis',(0.,0.,1.));
#10312=DIRECTION('ref_axis',(1.,-1.11022302462516E-15,0.));
#10313=DIRECTION('',(0.,0.,1.));
#10314=DIRECTION('center_axis',(1.,0.,0.));
#10315=DIRECTION('ref_axis',(0.,1.,0.));
#10316=DIRECTION('',(0.,1.,0.));
#10317=DIRECTION('',(0.,0.,1.));
#10318=DIRECTION('center_axis',(0.,0.,1.));
#10319=DIRECTION('ref_axis',(0.,-1.,0.));
#10320=DIRECTION('center_axis',(0.,0.,1.));
#10321=DIRECTION('ref_axis',(0.,-1.,0.));
#10322=DIRECTION('',(0.,0.,1.));
#10323=DIRECTION('center_axis',(-1.38777878078145E-16,-1.,0.));
#10324=DIRECTION('ref_axis',(1.,-1.38777878078145E-16,0.));
#10325=DIRECTION('',(1.,-1.38777878078145E-16,0.));
#10326=DIRECTION('',(0.,0.,1.));
#10327=DIRECTION('center_axis',(0.,0.,1.));
#10328=DIRECTION('ref_axis',(-1.,1.11022302462516E-15,0.));
#10329=DIRECTION('center_axis',(0.,0.,1.));
#10330=DIRECTION('ref_axis',(-1.,1.11022302462516E-15,0.));
#10331=DIRECTION('',(0.,0.,1.));
#10332=DIRECTION('center_axis',(-1.,0.,0.));
#10333=DIRECTION('ref_axis',(0.,-1.,0.));
#10334=DIRECTION('',(0.,-1.,0.));
#10335=DIRECTION('',(0.,0.,1.));
#10336=DIRECTION('center_axis',(0.,0.,1.));
#10337=DIRECTION('ref_axis',(1.11022302462516E-15,1.,0.));
#10338=DIRECTION('center_axis',(0.,0.,1.));
#10339=DIRECTION('ref_axis',(1.11022302462516E-15,1.,0.));
#10340=DIRECTION('center_axis',(0.,0.,1.));
#10341=DIRECTION('ref_axis',(1.,0.,0.));
#10342=DIRECTION('axis',(0.,0.,1.));
#10343=DIRECTION('refdir',(1.,0.,0.));
#10344=DIRECTION('center_axis',(0.,1.,0.));
#10345=DIRECTION('ref_axis',(0.707106781186555,0.,0.70710678118654));
#10346=DIRECTION('center_axis',(0.,1.,0.));
#10347=DIRECTION('ref_axis',(0.,0.,1.));
#10348=DIRECTION('',(0.,1.,0.));
#10349=DIRECTION('center_axis',(0.,-1.,0.));
#10350=DIRECTION('ref_axis',(1.,0.,0.));
#10351=DIRECTION('',(0.,-1.,0.));
#10352=DIRECTION('center_axis',(-1.,0.,0.));
#10353=DIRECTION('ref_axis',(0.,0.707106781186555,0.70710678118654));
#10354=DIRECTION('center_axis',(-1.,0.,0.));
#10355=DIRECTION('ref_axis',(0.,0.,1.));
#10356=DIRECTION('',(-1.,0.,0.));
#10357=DIRECTION('center_axis',(1.,-5.55111512312578E-16,0.));
#10358=DIRECTION('ref_axis',(5.55111512312578E-16,1.,0.));
#10359=DIRECTION('',(1.,0.,0.));
#10360=DIRECTION('center_axis',(0.408248290463862,0.40824829046386,-0.816496580927728));
#10361=DIRECTION('ref_axis',(0.577350269189629,0.577350269189628,0.577350269189621));
#10362=DIRECTION('center_axis',(0.,0.,1.));
#10363=DIRECTION('ref_axis',(1.,0.,0.));
#10364=DIRECTION('center_axis',(1.11022302462516E-16,-1.,0.));
#10365=DIRECTION('ref_axis',(-0.707106781186555,0.,0.70710678118654));
#10366=DIRECTION('center_axis',(0.,-1.,0.));
#10367=DIRECTION('ref_axis',(0.,0.,1.));
#10368=DIRECTION('',(1.11022302462516E-16,-1.,0.));
#10369=DIRECTION('center_axis',(0.,1.,0.));
#10370=DIRECTION('ref_axis',(-1.,0.,0.));
#10371=DIRECTION('',(-1.11022302462516E-16,1.,0.));
#10372=DIRECTION('center_axis',(-0.816496580927725,-0.408248290463869,-0.40824829046386));
#10373=DIRECTION('ref_axis',(-0.577350269189626,0.57735026918963,0.577350269189621));
#10374=DIRECTION('center_axis',(0.,0.,1.));
#10375=DIRECTION('ref_axis',(1.11022302462516E-15,1.,0.));
#10376=DIRECTION('center_axis',(1.,-2.22044604925031E-16,0.));
#10377=DIRECTION('ref_axis',(0.,-0.707106781186555,0.70710678118654));
#10378=DIRECTION('center_axis',(1.,0.,0.));
#10379=DIRECTION('ref_axis',(0.,0.,1.));
#10380=DIRECTION('',(1.,-2.22044604925031E-16,0.));
#10381=DIRECTION('center_axis',(-1.,0.,0.));
#10382=DIRECTION('ref_axis',(0.,-1.,0.));
#10383=DIRECTION('',(-1.,2.22044604925031E-16,0.));
#10384=DIRECTION('center_axis',(-0.816496580927724,0.408248290463871,-0.40824829046386));
#10385=DIRECTION('ref_axis',(-0.577350269189628,-0.577350269189629,0.577350269189621));
#10386=DIRECTION('center_axis',(0.,0.,1.));
#10387=DIRECTION('ref_axis',(-1.,0.,0.));
#10388=DIRECTION('center_axis',(-0.816496580927723,-0.408248290463872,0.408248290463859));
#10389=DIRECTION('ref_axis',(0.577350269189627,-0.577350269189631,0.57735026918962));
#10390=DIRECTION('center_axis',(0.,0.,1.));
#10391=DIRECTION('ref_axis',(5.55111512312576E-16,-1.,0.));
#10392=DIRECTION('center_axis',(0.,0.,1.));
#10393=DIRECTION('ref_axis',(1.,0.,0.));
#10394=DIRECTION('',(0.,0.,1.));
#10395=DIRECTION('center_axis',(0.,0.,1.));
#10396=DIRECTION('ref_axis',(1.,0.,0.));
#10397=DIRECTION('',(0.,0.,1.));
#10398=DIRECTION('center_axis',(1.,0.,0.));
#10399=DIRECTION('ref_axis',(0.,1.,0.));
#10400=DIRECTION('',(0.,0.,1.));
#10401=DIRECTION('',(0.,1.,0.));
#10402=DIRECTION('center_axis',(0.,0.,1.));
#10403=DIRECTION('ref_axis',(5.55111512312576E-16,-1.,0.));
#10404=DIRECTION('',(0.,0.,1.));
#10405=DIRECTION('center_axis',(0.,0.,1.));
#10406=DIRECTION('ref_axis',(5.55111512312576E-16,-1.,0.));
#10407=DIRECTION('center_axis',(-2.22044604925031E-16,-1.,0.));
#10408=DIRECTION('ref_axis',(1.,-2.22044604925031E-16,0.));
#10409=DIRECTION('',(0.,0.,1.));
#10410=DIRECTION('',(1.,-2.22044604925031E-16,0.));
#10411=DIRECTION('center_axis',(0.,0.,1.));
#10412=DIRECTION('ref_axis',(1.,0.,0.));
#10413=DIRECTION('center_axis',(0.,0.,-1.));
#10414=DIRECTION('ref_axis',(1.,0.,0.));
#10415=DIRECTION('center_axis',(0.0398594873598413,-0.995272787934818,-0.0885624009603703));
#10416=DIRECTION('ref_axis',(0.408479397061306,0.0971188838303287,-0.907586086594535));
#10417=DIRECTION('center_axis',(3.52448365596266E-13,1.77635683940025E-13,
-1.));
#10418=DIRECTION('ref_axis',(0.,1.,1.77635683940023E-13));
#10419=DIRECTION('center_axis',(0.892992097097124,0.450072343653862,0.));
#10420=DIRECTION('ref_axis',(-0.450072343653862,0.892992097097124,0.));
#10421=DIRECTION('center_axis',(1.,0.,0.));
#10422=DIRECTION('ref_axis',(0.,0.707106781186487,-0.707106781186609));
#10423=DIRECTION('center_axis',(0.,0.,1.));
#10424=DIRECTION('ref_axis',(0.97288028479796,0.231309211773851,0.));
#10425=DIRECTION('center_axis',(0.,0.,-1.));
#10426=DIRECTION('ref_axis',(0.,1.,0.));
#10427=DIRECTION('',(0.,0.,-1.));
#10428=DIRECTION('',(0.,-1.17758885217183E-15,1.));
#10429=DIRECTION('center_axis',(-0.775565134412812,-0.344096997179426,-0.529240945898311));
#10430=DIRECTION('ref_axis',(0.,0.838378187143696,-0.545088997615665));
#10431=DIRECTION('center_axis',(-0.775565134412822,0.344096997179426,0.529240945898297));
#10432=DIRECTION('ref_axis',(0.,0.838378187143689,-0.545088997615675));
#10433=DIRECTION('center_axis',(0.,-0.843786442012823,0.536679084998978));
#10434=DIRECTION('ref_axis',(0.,0.536679084998978,0.843786442012823));
#10435=DIRECTION('center_axis',(0.,0.838378187143685,-0.545088997615682));
#10436=DIRECTION('ref_axis',(0.,0.545088997615682,0.838378187143685));
#10437=DIRECTION('center_axis',(0.,0.,1.));
#10438=DIRECTION('ref_axis',(0.,1.,0.));
#10439=DIRECTION('center_axis',(0.,0.,-1.));
#10440=DIRECTION('ref_axis',(-0.97288028479796,0.231309211773851,0.));
#10441=DIRECTION('center_axis',(-7.89365027399415E-13,0.,1.));
#10442=DIRECTION('ref_axis',(0.,1.,0.));
#10443=DIRECTION('',(0.,0.,1.));
#10444=DIRECTION('',(0.,1.17758885217183E-15,-1.));
#10445=DIRECTION('center_axis',(-0.0398594873597966,-0.99527278793482,-0.0885624009603697));
#10446=DIRECTION('ref_axis',(-0.408479397061071,0.0971188838302721,-0.907586086594647));
#10447=DIRECTION('center_axis',(-1.,0.,0.));
#10448=DIRECTION('ref_axis',(0.,0.707106781186487,-0.707106781186609));
#10449=DIRECTION('center_axis',(-0.892992097097124,0.450072343653862,0.));
#10450=DIRECTION('ref_axis',(0.450072343653862,0.892992097097124,0.));
#10451=DIRECTION('center_axis',(0.,-1.,-1.17758885217183E-15));
#10452=DIRECTION('ref_axis',(0.,1.17758885217183E-15,-1.));
#10453=DIRECTION('',(1.,0.,0.));
#10454=DIRECTION('',(0.,-1.17758885217183E-15,1.));
#10455=DIRECTION('',(1.,0.,0.));
#10456=DIRECTION('center_axis',(1.,0.,0.));
#10457=DIRECTION('ref_axis',(0.,-0.83837818714366,0.54508899761572));
#10458=DIRECTION('',(-1.,0.,0.));
#10459=DIRECTION('center_axis',(-1.,0.,0.));
#10460=DIRECTION('ref_axis',(0.,-0.958743497277472,0.284272591763895));
#10461=DIRECTION('center_axis',(0.,-0.838378187143685,0.545088997615682));
#10462=DIRECTION('ref_axis',(0.,-0.545088997615682,-0.838378187143685));
#10463=DIRECTION('',(-1.,0.,0.));
#10464=DIRECTION('',(0.,-0.545088997615682,-0.838378187143685));
#10465=DIRECTION('',(1.,0.,0.));
#10466=DIRECTION('',(0.,0.545088997615682,0.838378187143685));
#10467=DIRECTION('center_axis',(1.,0.,0.));
#10468=DIRECTION('ref_axis',(0.,-0.83837818714366,0.54508899761572));
#10469=DIRECTION('',(1.,0.,0.));
#10470=DIRECTION('center_axis',(1.,0.,0.));
#10471=DIRECTION('ref_axis',(0.,-0.958743497277472,0.284272591763895));
#10472=DIRECTION('center_axis',(0.,-1.,-1.17758885217183E-15));
#10473=DIRECTION('ref_axis',(0.,1.17758885217183E-15,-1.));
#10474=DIRECTION('',(1.,0.,0.));
#10475=DIRECTION('',(0.,1.17758885217183E-15,-1.));
#10476=DIRECTION('center_axis',(1.,0.,0.));
#10477=DIRECTION('ref_axis',(0.,0.707106781186493,-0.707106781186602));
#10478=DIRECTION('',(-1.,0.,0.));
#10479=DIRECTION('center_axis',(-1.,0.,0.));
#10480=DIRECTION('ref_axis',(0.,1.,0.));
#10481=DIRECTION('center_axis',(0.,0.,1.));
#10482=DIRECTION('ref_axis',(-1.,-7.55896527404362E-16,0.));
#10483=DIRECTION('center_axis',(0.,0.,1.));
#10484=DIRECTION('ref_axis',(-1.,-1.01064309961486E-15,0.));
#10485=DIRECTION('center_axis',(0.,0.,1.));
#10486=DIRECTION('ref_axis',(-1.,-1.01064309961486E-15,0.));
#10487=DIRECTION('center_axis',(0.892992097097125,-0.450072343653861,0.));
#10488=DIRECTION('ref_axis',(-0.450072343653861,-0.892992097097125,0.));
#10489=DIRECTION('center_axis',(0.,0.,-1.));
#10490=DIRECTION('ref_axis',(-1.,-1.01064309961486E-15,0.));
#10491=DIRECTION('center_axis',(0.0398594873598144,-0.995272787934819,0.0885624009603698));
#10492=DIRECTION('ref_axis',(-0.408479397061211,-0.097118883830298,-0.907586086594581));
#10493=DIRECTION('center_axis',(3.52448365596266E-13,1.77635683940025E-13,
-1.));
#10494=DIRECTION('ref_axis',(0.,-1.,-1.7763568394003E-13));
#10495=DIRECTION('center_axis',(-0.892992097097125,-0.450072343653861,0.));
#10496=DIRECTION('ref_axis',(0.450072343653861,-0.892992097097125,0.));
#10497=DIRECTION('center_axis',(-1.,0.,0.));
#10498=DIRECTION('ref_axis',(0.,-0.707106781186636,-0.707106781186459));
#10499=DIRECTION('center_axis',(0.,0.,1.));
#10500=DIRECTION('ref_axis',(-0.972880284797955,-0.231309211773873,0.));
#10501=DIRECTION('center_axis',(0.,0.,-1.));
#10502=DIRECTION('ref_axis',(0.,-1.,0.));
#10503=DIRECTION('',(0.,0.,-1.));
#10504=DIRECTION('',(0.,1.17758885217183E-15,1.));
#10505=DIRECTION('center_axis',(0.775565134412811,0.344096997179419,-0.529240945898317));
#10506=DIRECTION('ref_axis',(0.,-0.838378187143704,-0.545088997615652));
#10507=DIRECTION('center_axis',(0.775565134412818,-0.344096997179424,0.529240945898304));
#10508=DIRECTION('ref_axis',(-2.77555756156297E-15,-0.838378187143696,-0.545088997615665));
#10509=DIRECTION('center_axis',(0.,0.843786442012823,0.536679084998978));
#10510=DIRECTION('ref_axis',(0.,-0.536679084998978,0.843786442012823));
#10511=DIRECTION('center_axis',(0.,-0.838378187143685,-0.545088997615682));
#10512=DIRECTION('ref_axis',(0.,-0.545088997615682,0.838378187143685));
#10513=DIRECTION('center_axis',(0.,0.,1.));
#10514=DIRECTION('ref_axis',(2.77555756156289E-15,-1.,0.));
#10515=DIRECTION('center_axis',(0.,0.,-1.));
#10516=DIRECTION('ref_axis',(0.97288028479796,-0.231309211773851,0.));
#10517=DIRECTION('center_axis',(0.,0.,1.));
#10518=DIRECTION('ref_axis',(0.,-1.,0.));
#10519=DIRECTION('',(0.,0.,1.));
#10520=DIRECTION('',(0.,-1.17758885217183E-15,-1.));
#10521=DIRECTION('center_axis',(-0.0398594873597704,-0.995272787934834,
0.0885624009602286));
#10522=DIRECTION('ref_axis',(0.408479397060976,-0.0971188838302492,-0.907586086594692));
#10523=DIRECTION('center_axis',(1.,0.,0.));
#10524=DIRECTION('ref_axis',(0.,-0.707106781186636,-0.707106781186459));
#10525=DIRECTION('center_axis',(0.,1.,-1.17758885217183E-15));
#10526=DIRECTION('ref_axis',(0.,1.17758885217183E-15,1.));
#10527=DIRECTION('',(1.,0.,0.));
#10528=DIRECTION('',(0.,1.17758885217183E-15,1.));
#10529=DIRECTION('',(-1.,0.,0.));
#10530=DIRECTION('center_axis',(1.,0.,0.));
#10531=DIRECTION('ref_axis',(0.,1.,-3.55271367880096E-14));
#10532=DIRECTION('',(1.,0.,0.));
#10533=DIRECTION('center_axis',(1.,0.,0.));
#10534=DIRECTION('ref_axis',(0.,0.958743497277472,0.284272591763895));
#10535=DIRECTION('center_axis',(0.,0.838378187143685,0.545088997615682));
#10536=DIRECTION('ref_axis',(0.,-0.545088997615682,0.838378187143685));
#10537=DIRECTION('',(1.,0.,0.));
#10538=DIRECTION('',(0.,0.545088997615682,-0.838378187143685));
#10539=DIRECTION('',(1.,0.,0.));
#10540=DIRECTION('',(0.,-0.545088997615682,0.838378187143685));
#10541=DIRECTION('center_axis',(1.,0.,0.));
#10542=DIRECTION('ref_axis',(0.,1.,-3.55271367880096E-14));
#10543=DIRECTION('',(1.,0.,0.));
#10544=DIRECTION('center_axis',(-1.,0.,0.));
#10545=DIRECTION('ref_axis',(0.,0.958743497277472,0.284272591763895));
#10546=DIRECTION('center_axis',(0.,1.,-1.17758885217183E-15));
#10547=DIRECTION('ref_axis',(0.,1.17758885217183E-15,1.));
#10548=DIRECTION('',(-1.,0.,0.));
#10549=DIRECTION('',(0.,-1.17758885217183E-15,-1.));
#10550=DIRECTION('center_axis',(-1.,0.,0.));
#10551=DIRECTION('ref_axis',(0.,-0.707106781186618,-0.707106781186477));
#10552=DIRECTION('',(1.,0.,0.));
#10553=DIRECTION('center_axis',(1.,0.,0.));
#10554=DIRECTION('ref_axis',(0.,-1.,0.));
#10555=DIRECTION('center_axis',(0.,0.,1.));
#10556=DIRECTION('ref_axis',(1.,0.,0.));
#10557=DIRECTION('center_axis',(0.,0.,-1.));
#10558=DIRECTION('ref_axis',(1.,-8.88178419700125E-16,0.));
#10559=DIRECTION('center_axis',(0.,0.,1.));
#10560=DIRECTION('ref_axis',(1.,-8.88178419700125E-16,0.));
#10561=DIRECTION('center_axis',(1.,0.,0.));
#10562=DIRECTION('ref_axis',(0.,0.707106781186493,-0.707106781186602));
#10563=DIRECTION('center_axis',(-1.,0.,0.));
#10564=DIRECTION('ref_axis',(0.,1.,0.));
#10565=DIRECTION('',(-1.,0.,0.));
#10566=DIRECTION('center_axis',(0.,1.,0.));
#10567=DIRECTION('ref_axis',(1.,0.,0.));
#10568=DIRECTION('center_axis',(0.,0.,1.));
#10569=DIRECTION('ref_axis',(0.707106781186546,0.707106781186549,0.));
#10570=DIRECTION('center_axis',(0.,0.,-1.));
#10571=DIRECTION('ref_axis',(0.707106781186546,0.707106781186549,0.));
#10572=DIRECTION('center_axis',(0.,-1.,0.));
#10573=DIRECTION('ref_axis',(0.707106781186618,0.,-0.707106781186477));
#10574=DIRECTION('center_axis',(5.55111512312578E-15,1.,0.));
#10575=DIRECTION('ref_axis',(1.,-5.55111512312578E-15,0.));
#10576=DIRECTION('',(0.,1.,0.));
#10577=DIRECTION('',(0.,-1.,0.));
#10578=DIRECTION('center_axis',(0.,0.,1.));
#10579=DIRECTION('ref_axis',(0.707106781186546,-0.707106781186549,0.));
#10580=DIRECTION('center_axis',(0.,0.,-1.));
#10581=DIRECTION('ref_axis',(0.707106781186546,-0.707106781186549,0.));
#10582=DIRECTION('center_axis',(0.,-1.17758885217183E-15,1.));
#10583=DIRECTION('ref_axis',(0.707106781186548,0.707106781186548,0.));
#10584=DIRECTION('center_axis',(0.,0.,-1.));
#10585=DIRECTION('ref_axis',(0.,1.,0.));
#10586=DIRECTION('',(0.,1.17758885217183E-15,-1.));
#10587=DIRECTION('center_axis',(0.,0.,1.));
#10588=DIRECTION('ref_axis',(1.,0.,0.));
#10589=DIRECTION('',(0.,0.,-1.));
#10590=DIRECTION('center_axis',(0.,0.,1.));
#10591=DIRECTION('ref_axis',(1.,0.,0.));
#10592=DIRECTION('center_axis',(-1.,0.,0.));
#10593=DIRECTION('ref_axis',(0.,-0.707106781186618,-0.707106781186477));
#10594=DIRECTION('center_axis',(1.,0.,0.));
#10595=DIRECTION('ref_axis',(0.,-1.,0.));
#10596=DIRECTION('',(1.,0.,0.));
#10597=DIRECTION('center_axis',(0.,-1.,0.));
#10598=DIRECTION('ref_axis',(-1.,0.,0.));
#10599=DIRECTION('center_axis',(0.,0.,1.));
#10600=DIRECTION('ref_axis',(-0.707106781186546,-0.707106781186549,0.));
#10601=DIRECTION('center_axis',(0.,0.,-1.));
#10602=DIRECTION('ref_axis',(-0.707106781186546,-0.707106781186549,0.));
#10603=DIRECTION('center_axis',(0.,1.,0.));
#10604=DIRECTION('ref_axis',(-0.707106781186618,0.,-0.707106781186477));
#10605=DIRECTION('center_axis',(5.55111512312578E-15,-1.,0.));
#10606=DIRECTION('ref_axis',(-1.,-5.55111512312578E-15,0.));
#10607=DIRECTION('',(0.,-1.,0.));
#10608=DIRECTION('',(0.,1.,0.));
#10609=DIRECTION('center_axis',(0.,0.,1.));
#10610=DIRECTION('ref_axis',(-0.707106781186546,0.707106781186549,0.));
#10611=DIRECTION('center_axis',(0.,0.,-1.));
#10612=DIRECTION('ref_axis',(-0.707106781186546,0.707106781186549,0.));
#10613=DIRECTION('center_axis',(0.,1.17758885217183E-15,1.));
#10614=DIRECTION('ref_axis',(-0.707106781186548,-0.707106781186548,0.));
#10615=DIRECTION('center_axis',(0.,0.,-1.));
#10616=DIRECTION('ref_axis',(0.,-1.,0.));
#10617=DIRECTION('',(0.,-1.17758885217183E-15,-1.));
#10618=DIRECTION('center_axis',(0.,0.,1.));
#10619=DIRECTION('ref_axis',(1.,0.,0.));
#10620=DIRECTION('center_axis',(0.,0.545088997615682,-0.838378187143685));
#10621=DIRECTION('ref_axis',(0.707106781186562,-0.592822901328176,-0.385436126564212));
#10622=DIRECTION('center_axis',(0.,0.545088997615662,-0.838378187143697));
#10623=DIRECTION('ref_axis',(1.,0.,0.));
#10624=DIRECTION('center_axis',(0.,-0.545088997615661,0.838378187143698));
#10625=DIRECTION('ref_axis',(0.,-0.838378187143698,-0.545088997615661));
#10626=DIRECTION('',(0.,-0.545088997615682,0.838378187143685));
#10627=DIRECTION('center_axis',(-1.,0.,0.));
#10628=DIRECTION('ref_axis',(0.,0.,1.));
#10629=DIRECTION('center_axis',(0.,0.,1.));
#10630=DIRECTION('ref_axis',(0.,-1.,0.));
#10631=DIRECTION('center_axis',(1.,0.,0.));
#10632=DIRECTION('ref_axis',(0.,0.958743497277472,0.284272591763895));
#10633=DIRECTION('center_axis',(0.,-1.17758885217183E-15,-1.));
#10634=DIRECTION('ref_axis',(0.707106781186548,-0.707106781186548,0.));
#10635=DIRECTION('',(0.,1.17758885217183E-15,1.));
#10636=DIRECTION('center_axis',(-2.95822839457884E-27,8.88178419700139E-14,
-1.));
#10637=DIRECTION('ref_axis',(1.,3.33066907387547E-14,0.));
#10638=DIRECTION('center_axis',(1.,0.,0.));
#10639=DIRECTION('ref_axis',(0.,-0.424803640464789,-0.905285516866288));
#10640=DIRECTION('center_axis',(-1.,0.,0.));
#10641=DIRECTION('ref_axis',(0.,-0.424803640464789,-0.905285516866288));
#10642=DIRECTION('center_axis',(1.,0.,0.));
#10643=DIRECTION('ref_axis',(0.,-1.,0.));
#10644=DIRECTION('center_axis',(1.,0.,0.));
#10645=DIRECTION('ref_axis',(0.,-0.958743497277472,0.284272591763895));
#10646=DIRECTION('',(0.,-0.545088997615682,-0.838378187143685));
#10647=DIRECTION('center_axis',(-1.,0.,0.));
#10648=DIRECTION('ref_axis',(0.,0.424803640464811,-0.905285516866278));
#10649=DIRECTION('',(0.,0.,-1.));
#10650=DIRECTION('',(0.,1.,0.));
#10651=DIRECTION('',(0.,0.,-1.));
#10652=DIRECTION('center_axis',(-1.,0.,0.));
#10653=DIRECTION('ref_axis',(0.,1.,0.));
#10654=DIRECTION('',(0.,-1.,0.));
#10655=DIRECTION('center_axis',(-1.,0.,0.));
#10656=DIRECTION('ref_axis',(0.,0.,1.));
#10657=DIRECTION('center_axis',(0.,-0.545088997615734,-0.838378187143651));
#10658=DIRECTION('ref_axis',(0.,0.838378187143651,-0.545088997615734));
#10659=DIRECTION('center_axis',(0.,0.545088997615682,0.838378187143685));
#10660=DIRECTION('ref_axis',(0.707106781186561,0.592822901328178,-0.385436126564211));
#10661=DIRECTION('center_axis',(0.,-0.545088997615661,-0.838378187143698));
#10662=DIRECTION('ref_axis',(0.,0.838378187143698,-0.545088997615661));
#10663=DIRECTION('center_axis',(0.,0.,-1.));
#10664=DIRECTION('ref_axis',(5.55111512312587E-15,1.,0.));
#10665=DIRECTION('center_axis',(1.,0.,0.));
#10666=DIRECTION('ref_axis',(0.,0.424803640464811,-0.905285516866278));
#10667=DIRECTION('center_axis',(0.,-0.545088997615682,-0.838378187143685));
#10668=DIRECTION('ref_axis',(-0.707106781186561,0.592822901328178,-0.385436126564211));
#10669=DIRECTION('center_axis',(0.,-0.545088997615662,-0.838378187143697));
#10670=DIRECTION('ref_axis',(-1.,0.,0.));
#10671=DIRECTION('center_axis',(0.,0.545088997615662,0.838378187143697));
#10672=DIRECTION('ref_axis',(0.,0.838378187143697,-0.545088997615662));
#10673=DIRECTION('',(0.,0.545088997615682,0.838378187143685));
#10674=DIRECTION('center_axis',(1.,0.,0.));
#10675=DIRECTION('ref_axis',(0.,0.,-1.));
#10676=DIRECTION('center_axis',(0.,0.,1.));
#10677=DIRECTION('ref_axis',(0.,1.,0.));
#10678=DIRECTION('center_axis',(-1.,0.,0.));
#10679=DIRECTION('ref_axis',(0.,-0.958743497277472,0.284272591763895));
#10680=DIRECTION('center_axis',(0.,1.17758885217183E-15,-1.));
#10681=DIRECTION('ref_axis',(-0.707106781186548,0.707106781186548,0.));
#10682=DIRECTION('',(0.,-1.17758885217183E-15,1.));
#10683=DIRECTION('center_axis',(0.,0.,-1.));
#10684=DIRECTION('ref_axis',(-1.,-2.22044604925031E-14,0.));
#10685=DIRECTION('center_axis',(-1.,0.,0.));
#10686=DIRECTION('ref_axis',(0.,0.424803640464792,-0.905285516866286));
#10687=DIRECTION('center_axis',(1.,0.,0.));
#10688=DIRECTION('ref_axis',(0.,0.424803640464792,-0.905285516866286));
#10689=DIRECTION('center_axis',(-1.,0.,0.));
#10690=DIRECTION('ref_axis',(0.,1.,0.));
#10691=DIRECTION('center_axis',(-1.,0.,0.));
#10692=DIRECTION('ref_axis',(0.,0.958743497277472,0.284272591763895));
#10693=DIRECTION('',(0.,0.545088997615682,-0.838378187143685));
#10694=DIRECTION('center_axis',(1.,0.,0.));
#10695=DIRECTION('ref_axis',(0.,-0.424803640464792,-0.905285516866286));
#10696=DIRECTION('',(0.,0.,-1.));
#10697=DIRECTION('',(0.,-1.,0.));
#10698=DIRECTION('',(0.,0.,-1.));
#10699=DIRECTION('',(0.,1.,0.));
#10700=DIRECTION('center_axis',(1.,0.,0.));
#10701=DIRECTION('ref_axis',(0.,1.,0.));
#10702=DIRECTION('center_axis',(1.,0.,0.));
#10703=DIRECTION('ref_axis',(0.,0.,-1.));
#10704=DIRECTION('center_axis',(0.,0.545088997615732,-0.838378187143652));
#10705=DIRECTION('ref_axis',(0.,-0.838378187143652,-0.545088997615732));
#10706=DIRECTION('center_axis',(0.,-0.545088997615682,0.838378187143685));
#10707=DIRECTION('ref_axis',(-0.707106781186561,-0.592822901328178,-0.385436126564211));
#10708=DIRECTION('center_axis',(0.,0.545088997615661,-0.838378187143698));
#10709=DIRECTION('ref_axis',(0.,-0.838378187143698,-0.545088997615661));
#10710=DIRECTION('center_axis',(-8.88178419700124E-14,0.,-1.));
#10711=DIRECTION('ref_axis',(0.,-1.,0.));
#10712=DIRECTION('center_axis',(-1.,0.,0.));
#10713=DIRECTION('ref_axis',(0.,-0.424803640464792,-0.905285516866286));
#10714=DIRECTION('center_axis',(1.,0.,0.));
#10715=DIRECTION('ref_axis',(0.,0.838378187143673,-0.545088997615699));
#10716=DIRECTION('',(-1.,0.,0.));
#10717=DIRECTION('center_axis',(1.,0.,0.));
#10718=DIRECTION('ref_axis',(0.,-1.,-4.4408920985003E-14));
#10719=DIRECTION('',(-1.,0.,0.));
#10720=DIRECTION('center_axis',(0.,1.,0.));
#10721=DIRECTION('ref_axis',(1.,0.,0.));
#10722=DIRECTION('',(0.,0.,-1.));
#10723=DIRECTION('',(-1.,0.,0.));
#10724=DIRECTION('',(0.,0.,-1.));
#10725=DIRECTION('center_axis',(-1.11022302462516E-16,-1.,0.));
#10726=DIRECTION('ref_axis',(-1.,1.11022302462516E-16,0.));
#10727=DIRECTION('',(0.,0.,-1.));
#10728=DIRECTION('',(1.,-1.11022302462516E-16,0.));
#10729=DIRECTION('',(0.,0.,-1.));
#10730=DIRECTION('center_axis',(1.,0.,0.));
#10731=DIRECTION('ref_axis',(0.,-8.26946079742758E-16,1.));
#10732=DIRECTION('',(1.,0.,0.));
#10733=DIRECTION('center_axis',(1.,0.,0.));
#10734=DIRECTION('ref_axis',(0.,1.,0.));
#10735=DIRECTION('',(-1.,0.,0.));
#10736=DIRECTION('center_axis',(0.,0.,-1.));
#10737=DIRECTION('ref_axis',(0.,1.,0.));
#10738=DIRECTION('',(0.,1.,0.));
#10739=DIRECTION('center_axis',(1.,0.,0.));
#10740=DIRECTION('ref_axis',(0.,1.,0.));
#10741=DIRECTION('center_axis',(0.,0.,-1.));
#10742=DIRECTION('ref_axis',(0.,1.,0.));
#10743=DIRECTION('',(1.,0.,0.));
#10744=DIRECTION('',(0.,-1.,0.));
#10745=DIRECTION('',(-1.,0.,0.));
#10746=DIRECTION('center_axis',(1.,0.,0.));
#10747=DIRECTION('ref_axis',(0.,1.,0.));
#10748=DIRECTION('center_axis',(-1.,0.,0.));
#10749=DIRECTION('ref_axis',(0.,1.,0.));
#10750=DIRECTION('center_axis',(1.,0.,0.));
#10751=DIRECTION('ref_axis',(0.,-8.26946079742758E-16,1.));
#10752=DIRECTION('center_axis',(0.,0.,-1.));
#10753=DIRECTION('ref_axis',(0.,1.,0.));
#10754=DIRECTION('center_axis',(0.,0.,1.));
#10755=DIRECTION('ref_axis',(0.,1.,0.));
#10756=DIRECTION('center_axis',(0.,0.,-1.));
#10757=DIRECTION('ref_axis',(-1.,-5.55111512312578E-15,0.));
#10758=DIRECTION('center_axis',(0.,0.,1.));
#10759=DIRECTION('ref_axis',(-1.,-5.55111512312578E-15,0.));
#10760=DIRECTION('center_axis',(0.,0.,-1.));
#10761=DIRECTION('ref_axis',(2.77555756156287E-15,-1.,0.));
#10762=DIRECTION('center_axis',(0.,0.,1.));
#10763=DIRECTION('ref_axis',(2.77555756156287E-15,-1.,0.));
#10764=DIRECTION('center_axis',(0.,0.,-1.));
#10765=DIRECTION('ref_axis',(1.,5.55111512312578E-15,0.));
#10766=DIRECTION('center_axis',(0.,0.,1.));
#10767=DIRECTION('ref_axis',(1.,5.55111512312578E-15,0.));
#10768=DIRECTION('center_axis',(0.,0.,1.));
#10769=DIRECTION('ref_axis',(-1.,0.,0.));
#10770=DIRECTION('',(0.,0.,1.));
#10771=DIRECTION('center_axis',(0.,0.,1.));
#10772=DIRECTION('ref_axis',(-1.,0.,0.));
#10773=DIRECTION('center_axis',(-1.,-1.11022302462516E-16,0.));
#10774=DIRECTION('ref_axis',(1.11022302462516E-16,-1.,0.));
#10775=DIRECTION('',(0.,0.,1.));
#10776=DIRECTION('',(1.11022302462516E-16,-1.,0.));
#10777=DIRECTION('center_axis',(0.,0.,1.));
#10778=DIRECTION('ref_axis',(1.11022302462516E-15,1.,0.));
#10779=DIRECTION('',(0.,0.,1.));
#10780=DIRECTION('center_axis',(0.,0.,1.));
#10781=DIRECTION('ref_axis',(1.11022302462516E-15,1.,0.));
#10782=DIRECTION('center_axis',(0.,1.,0.));
#10783=DIRECTION('ref_axis',(-1.,0.,0.));
#10784=DIRECTION('',(-1.,0.,0.));
#10785=DIRECTION('center_axis',(0.,0.,1.));
#10786=DIRECTION('ref_axis',(1.,0.,0.));
#10787=DIRECTION('axis',(0.,0.,1.));
#10788=DIRECTION('refdir',(1.,0.,0.));
#10789=DIRECTION('center_axis',(0.,0.,-1.));
#10790=DIRECTION('ref_axis',(-1.,0.,0.));
#10791=DIRECTION('center_axis',(0.,0.,-1.));
#10792=DIRECTION('ref_axis',(-1.,0.,0.));
#10793=DIRECTION('',(-0.707106781186542,8.65956056235487E-17,0.707106781186553));
#10794=DIRECTION('center_axis',(0.,0.,1.));
#10795=DIRECTION('ref_axis',(-1.,0.,0.));
#10796=DIRECTION('center_axis',(0.,0.,1.));
#10797=DIRECTION('ref_axis',(-1.,0.,0.));
#10798=DIRECTION('center_axis',(0.,0.,-1.));
#10799=DIRECTION('ref_axis',(-1.,0.,0.));
#10800=DIRECTION('',(0.,0.,-1.));
#10801=DIRECTION('center_axis',(0.,0.,-1.));
#10802=DIRECTION('ref_axis',(-1.,0.,0.));
#10803=DIRECTION('center_axis',(0.,0.,-1.));
#10804=DIRECTION('ref_axis',(-1.,0.,0.));
#10805=DIRECTION('center_axis',(0.,0.,1.));
#10806=DIRECTION('ref_axis',(-1.,0.,0.));
#10807=DIRECTION('center_axis',(0.,0.,1.));
#10808=DIRECTION('ref_axis',(-1.,0.,0.));
#10809=DIRECTION('',(-0.707106781186542,-8.65956056235487E-17,-0.707106781186553));
#10810=DIRECTION('center_axis',(0.,0.,-1.));
#10811=DIRECTION('ref_axis',(-1.,0.,0.));
#10812=DIRECTION('center_axis',(0.,0.,1.));
#10813=DIRECTION('ref_axis',(-1.,0.,0.));
#10814=DIRECTION('center_axis',(0.,0.,1.));
#10815=DIRECTION('ref_axis',(-1.,0.,0.));
#10816=DIRECTION('',(0.,0.,-1.));
#10817=DIRECTION('axis',(0.,0.,1.));
#10818=DIRECTION('refdir',(1.,0.,0.));
#10819=DIRECTION('center_axis',(0.,0.,1.));
#10820=DIRECTION('ref_axis',(-0.651162790697674,0.758938087073522,0.));
#10821=DIRECTION('center_axis',(-0.667972400760236,-0.744186046511628,0.));
#10822=DIRECTION('ref_axis',(0.,0.,1.));
#10823=DIRECTION('center_axis',(0.,0.,1.));
#10824=DIRECTION('ref_axis',(-1.,0.,0.));
#10825=DIRECTION('center_axis',(-0.667972400760235,0.744186046511629,5.98505826505541E-15));
#10826=DIRECTION('ref_axis',(-0.744186046511629,-0.667972400760235,0.));
#10827=DIRECTION('center_axis',(0.,0.,1.));
#10828=DIRECTION('ref_axis',(-0.908615097469131,0.417634534792277,0.));
#10829=DIRECTION('center_axis',(0.,0.,-1.));
#10830=DIRECTION('ref_axis',(-1.,0.,0.));
#10831=DIRECTION('',(0.,0.,-1.));
#10832=DIRECTION('',(0.,0.,1.));
#10833=DIRECTION('center_axis',(0.,1.,1.80411241501592E-14));
#10834=DIRECTION('ref_axis',(-1.,0.,0.));
#10835=DIRECTION('center_axis',(-2.01858731750028E-16,-1.,0.));
#10836=DIRECTION('ref_axis',(-0.707106781186618,0.,0.707106781186477));
#10837=DIRECTION('center_axis',(0.,1.,1.38777878078148E-15));
#10838=DIRECTION('ref_axis',(-1.,0.,0.));
#10839=DIRECTION('',(2.01858731750028E-16,1.,0.));
#10840=DIRECTION('',(-2.01858731750028E-16,-1.,0.));
#10841=DIRECTION('center_axis',(0.,0.,1.));
#10842=DIRECTION('ref_axis',(-1.,-2.77555756156289E-15,0.));
#10843=DIRECTION('center_axis',(0.,0.,-1.));
#10844=DIRECTION('ref_axis',(-0.90861509746913,-0.417634534792279,0.));
#10845=DIRECTION('',(0.,0.,1.));
#10846=DIRECTION('',(0.,0.,-1.));
#10847=DIRECTION('center_axis',(-2.01858731750028E-16,-1.,0.));
#10848=DIRECTION('ref_axis',(0.707106781186493,0.,-0.707106781186602));
#10849=DIRECTION('',(2.01858731750028E-16,1.,0.));
#10850=DIRECTION('',(-2.01858731750028E-16,-1.,0.));
#10851=DIRECTION('center_axis',(0.,0.,-1.));
#10852=DIRECTION('ref_axis',(-1.,0.,0.));
#10853=DIRECTION('center_axis',(0.,0.,1.));
#10854=DIRECTION('ref_axis',(-1.,-1.22464679914735E-16,0.));
#10855=DIRECTION('center_axis',(0.,0.,1.));
#10856=DIRECTION('ref_axis',(-1.,-1.22464679914735E-16,0.));
#10857=DIRECTION('center_axis',(0.,0.,-1.));
#10858=DIRECTION('ref_axis',(-1.,-1.22464679914735E-16,0.));
#10859=DIRECTION('center_axis',(0.,0.,1.));
#10860=DIRECTION('ref_axis',(1.,0.,0.));
#10861=DIRECTION('center_axis',(0.,0.,-1.));
#10862=DIRECTION('ref_axis',(6.12323399573677E-17,-1.,0.));
#10863=DIRECTION('',(-1.51394048812521E-16,-1.,0.));
#10864=DIRECTION('center_axis',(0.,0.,-1.));
#10865=DIRECTION('ref_axis',(5.0532154980743E-16,1.,0.));
#10866=DIRECTION('center_axis',(0.,0.,1.));
#10867=DIRECTION('ref_axis',(1.,0.,0.));
#10868=DIRECTION('center_axis',(0.,0.,1.));
#10869=DIRECTION('ref_axis',(6.12323399573677E-17,-1.,0.));
#10870=DIRECTION('center_axis',(1.,-2.01858731750028E-16,0.));
#10871=DIRECTION('ref_axis',(-2.01858731750028E-16,-1.,0.));
#10872=DIRECTION('center_axis',(1.,-2.01858731750028E-16,0.));
#10873=DIRECTION('ref_axis',(0.,-1.,0.));
#10874=DIRECTION('center_axis',(0.,0.,1.));
#10875=DIRECTION('ref_axis',(-1.,0.,0.));
#10876=DIRECTION('center_axis',(0.,0.,1.));
#10877=DIRECTION('ref_axis',(1.,0.,0.));
#10878=DIRECTION('center_axis',(0.667972400760235,-0.744186046511629,-2.06553120860499E-15));
#10879=DIRECTION('ref_axis',(0.744186046511629,0.667972400760235,0.));
#10880=DIRECTION('center_axis',(0.,0.,1.));
#10881=DIRECTION('ref_axis',(0.651162790697674,-0.758938087073522,0.));
#10882=DIRECTION('center_axis',(0.667972400760231,0.744186046511633,0.));
#10883=DIRECTION('ref_axis',(0.,0.,1.));
#10884=DIRECTION('center_axis',(0.,0.,1.));
#10885=DIRECTION('ref_axis',(0.90861509746913,-0.417634534792279,0.));
#10886=DIRECTION('center_axis',(0.,0.,-1.));
#10887=DIRECTION('ref_axis',(1.,0.,0.));
#10888=DIRECTION('',(0.,0.,-1.));
#10889=DIRECTION('',(0.,0.,1.));
#10890=DIRECTION('center_axis',(0.,-1.,2.9143354396411E-14));
#10891=DIRECTION('ref_axis',(1.,0.,0.));
#10892=DIRECTION('center_axis',(1.51394048812521E-16,1.,0.));
#10893=DIRECTION('ref_axis',(0.707106781186618,0.,0.707106781186477));
#10894=DIRECTION('center_axis',(0.,-1.,0.));
#10895=DIRECTION('ref_axis',(1.,0.,0.));
#10896=DIRECTION('',(1.51394048812521E-16,1.,0.));
#10897=DIRECTION('center_axis',(0.,0.,1.));
#10898=DIRECTION('ref_axis',(1.,2.77555756156289E-15,0.));
#10899=DIRECTION('center_axis',(0.,0.,-1.));
#10900=DIRECTION('ref_axis',(0.90861509746913,0.417634534792279,0.));
#10901=DIRECTION('',(0.,0.,1.));
#10902=DIRECTION('',(0.,0.,-1.));
#10903=DIRECTION('center_axis',(0.,0.,-1.));
#10904=DIRECTION('ref_axis',(1.,-9.86864910777917E-17,0.));
#10905=DIRECTION('center_axis',(0.,0.,1.));
#10906=DIRECTION('ref_axis',(1.,-5.55111512312578E-17,0.));
#10907=DIRECTION('center_axis',(0.,0.,-1.));
#10908=DIRECTION('ref_axis',(1.,-5.55111512312578E-17,0.));
#10909=DIRECTION('center_axis',(1.51394048812521E-16,1.,0.));
#10910=DIRECTION('ref_axis',(-0.707106781186493,0.,-0.707106781186602));
#10911=DIRECTION('',(-1.51394048812521E-16,-1.,0.));
#10912=DIRECTION('',(1.51394048812521E-16,1.,0.));
#10913=DIRECTION('center_axis',(0.,0.,1.));
#10914=DIRECTION('ref_axis',(1.,0.,0.));
#10915=DIRECTION('center_axis',(0.,0.,1.));
#10916=DIRECTION('ref_axis',(5.0532154980743E-16,1.,0.));
#10917=DIRECTION('',(0.,0.,-1.));
#10918=DIRECTION('center_axis',(0.,0.,-1.));
#10919=DIRECTION('ref_axis',(1.,0.,0.));
#10920=DIRECTION('center_axis',(-1.,1.51394048812521E-16,0.));
#10921=DIRECTION('ref_axis',(1.51394048812521E-16,1.,0.));
#10922=DIRECTION('center_axis',(-1.,1.51394048812521E-16,0.));
#10923=DIRECTION('ref_axis',(0.,-1.,0.));
#10924=DIRECTION('center_axis',(0.,0.,1.));
#10925=DIRECTION('ref_axis',(-1.,0.,0.));
#10926=DIRECTION('center_axis',(0.,0.,1.));
#10927=DIRECTION('ref_axis',(1.,0.,0.));
#10928=DIRECTION('center_axis',(0.,0.,1.));
#10929=DIRECTION('ref_axis',(1.,0.,0.));
#10930=DIRECTION('center_axis',(1.2335811384724E-16,-1.,0.));
#10931=DIRECTION('ref_axis',(-1.,-1.2335811384724E-16,0.));
#10932=DIRECTION('center_axis',(0.,0.,1.));
#10933=DIRECTION('ref_axis',(1.,0.,0.));
#10934=DIRECTION('center_axis',(0.,0.,1.));
#10935=DIRECTION('ref_axis',(1.,0.,0.));
#10936=DIRECTION('center_axis',(0.,0.,-1.));
#10937=DIRECTION('ref_axis',(1.,0.,0.));
#10938=DIRECTION('center_axis',(0.,0.,1.));
#10939=DIRECTION('ref_axis',(1.,0.,0.));
#10940=DIRECTION('center_axis',(0.,0.,1.));
#10941=DIRECTION('ref_axis',(1.,0.,0.));
#10942=DIRECTION('center_axis',(1.42336285208353E-16,-1.,0.));
#10943=DIRECTION('ref_axis',(-1.,-1.42336285208353E-16,0.));
#10944=DIRECTION('center_axis',(0.,0.,-1.));
#10945=DIRECTION('ref_axis',(1.,0.,0.));
#10946=DIRECTION('center_axis',(0.,0.,-1.));
#10947=DIRECTION('ref_axis',(1.,0.,0.));
#10948=DIRECTION('',(0.,0.,1.));
#10949=DIRECTION('center_axis',(0.,0.,-1.));
#10950=DIRECTION('ref_axis',(1.,0.,0.));
#10951=DIRECTION('center_axis',(0.,0.,-1.));
#10952=DIRECTION('ref_axis',(-1.,0.,0.));
#10953=DIRECTION('center_axis',(0.,0.,1.));
#10954=DIRECTION('ref_axis',(1.,0.,0.));
#10955=DIRECTION('center_axis',(-1.58603289232165E-16,-1.,0.));
#10956=DIRECTION('ref_axis',(1.,-1.58603289232165E-16,0.));
#10957=DIRECTION('center_axis',(0.,0.,1.));
#10958=DIRECTION('ref_axis',(1.,0.,0.));
#10959=DIRECTION('center_axis',(0.,0.,-1.));
#10960=DIRECTION('ref_axis',(1.,0.,0.));
#10961=DIRECTION('center_axis',(0.,0.,-1.));
#10962=DIRECTION('ref_axis',(1.,0.,0.));
#10963=DIRECTION('',(0.707106781186542,-8.65956056235487E-17,0.707106781186553));
#10964=DIRECTION('center_axis',(0.,0.,1.));
#10965=DIRECTION('ref_axis',(1.,0.,0.));
#10966=DIRECTION('center_axis',(0.,0.,-1.));
#10967=DIRECTION('ref_axis',(1.,0.,0.));
#10968=DIRECTION('',(0.,0.,1.));
#10969=DIRECTION('center_axis',(0.,0.,-1.));
#10970=DIRECTION('ref_axis',(1.,0.,0.));
#10971=DIRECTION('center_axis',(1.,0.,0.));
#10972=DIRECTION('ref_axis',(0.,-1.,0.));
#10973=DIRECTION('',(1.,0.,0.));
#10974=DIRECTION('center_axis',(0.,0.,1.));
#10975=DIRECTION('ref_axis',(1.,0.,0.));
#10976=DIRECTION('axis',(0.,0.,1.));
#10977=DIRECTION('refdir',(1.,0.,0.));
#10978=DIRECTION('center_axis',(0.,0.,-1.));
#10979=DIRECTION('ref_axis',(1.,0.,0.));
#10980=DIRECTION('',(0.,0.,1.));
#10981=DIRECTION('center_axis',(0.,0.,-1.));
#10982=DIRECTION('ref_axis',(1.,0.,0.));
#10983=DIRECTION('center_axis',(0.,0.,-1.));
#10984=DIRECTION('ref_axis',(1.,0.,0.));
#10985=DIRECTION('',(0.,0.,1.));
#10986=DIRECTION('center_axis',(0.,0.,-1.));
#10987=DIRECTION('ref_axis',(1.,0.,0.));
#10988=DIRECTION('',(0.,0.,1.));
#10989=DIRECTION('center_axis',(0.,0.,-1.));
#10990=DIRECTION('ref_axis',(1.,0.,0.));
#10991=DIRECTION('',(0.,0.,1.));
#10992=DIRECTION('center_axis',(0.,0.,-1.));
#10993=DIRECTION('ref_axis',(1.,0.,0.));
#10994=DIRECTION('',(0.,0.,1.));
#10995=DIRECTION('center_axis',(0.,0.,-1.));
#10996=DIRECTION('ref_axis',(1.,0.,0.));
#10997=DIRECTION('',(0.,0.,1.));
#10998=DIRECTION('center_axis',(0.,0.,-1.));
#10999=DIRECTION('ref_axis',(0.986989031429609,0.160787598519419,0.));
#11000=DIRECTION('',(0.,0.,-1.));
#11001=DIRECTION('center_axis',(0.,0.,-1.));
#11002=DIRECTION('ref_axis',(1.,-4.52218161043494E-15,0.));
#11003=DIRECTION('center_axis',(0.,0.,-1.));
#11004=DIRECTION('ref_axis',(1.,-4.52218161043494E-15,0.));
#11005=DIRECTION('',(0.,0.,-1.));
#11006=DIRECTION('center_axis',(0.,0.,-1.));
#11007=DIRECTION('ref_axis',(1.,-4.52218161043494E-15,0.));
#11008=DIRECTION('',(0.,0.,-1.));
#11009=DIRECTION('center_axis',(0.,0.,-1.));
#11010=DIRECTION('ref_axis',(1.,-4.52218161043494E-15,0.));
#11011=DIRECTION('',(0.,0.,-1.));
#11012=DIRECTION('center_axis',(0.,0.,-1.));
#11013=DIRECTION('ref_axis',(1.,-4.52218161043494E-15,0.));
#11014=DIRECTION('',(0.,0.,-1.));
#11015=DIRECTION('center_axis',(0.,0.,-1.));
#11016=DIRECTION('ref_axis',(1.,-4.52218161043494E-15,0.));
#11017=DIRECTION('center_axis',(0.,0.,1.));
#11018=DIRECTION('ref_axis',(1.,-4.52218161043494E-15,0.));
#11019=DIRECTION('center_axis',(0.,0.,1.));
#11020=DIRECTION('ref_axis',(1.,0.,0.));
#11021=DIRECTION('center_axis',(0.,0.,-1.));
#11022=DIRECTION('ref_axis',(1.,0.,0.));
#11023=DIRECTION('center_axis',(0.,0.,-1.));
#11024=DIRECTION('ref_axis',(1.,0.,0.));
#11025=DIRECTION('center_axis',(0.,0.,-1.));
#11026=DIRECTION('ref_axis',(1.,0.,0.));
#11027=DIRECTION('center_axis',(0.,0.,-1.));
#11028=DIRECTION('ref_axis',(1.,0.,0.));
#11029=DIRECTION('',(0.,0.,1.));
#11030=DIRECTION('center_axis',(0.,0.,1.));
#11031=DIRECTION('ref_axis',(1.,0.,0.));
#11032=DIRECTION('center_axis',(0.,0.,1.));
#11033=DIRECTION('ref_axis',(1.,0.,0.));
#11034=DIRECTION('center_axis',(0.,0.,1.));
#11035=DIRECTION('ref_axis',(1.,0.,0.));
#11036=DIRECTION('center_axis',(0.,0.,1.));
#11037=DIRECTION('ref_axis',(1.,0.,0.));
#11038=DIRECTION('center_axis',(0.,0.,-1.));
#11039=DIRECTION('ref_axis',(1.,0.,0.));
#11040=DIRECTION('',(0.,0.,1.));
#11041=DIRECTION('center_axis',(0.,0.,-1.));
#11042=DIRECTION('ref_axis',(-0.23846786087739,0.971150389655774,0.));
#11043=DIRECTION('axis',(0.,0.,1.));
#11044=DIRECTION('refdir',(1.,0.,0.));
#11045=DIRECTION('center_axis',(-0.980580675690919,-0.196116135138188,0.));
#11046=DIRECTION('ref_axis',(-0.196116135138188,0.980580675690919,0.));
#11047=DIRECTION('center_axis',(0.196116135138188,0.980580675690919,0.));
#11048=DIRECTION('ref_axis',(-0.980580675690919,0.196116135138188,0.));
#11049=DIRECTION('center_axis',(0.,0.,-1.));
#11050=DIRECTION('ref_axis',(-1.,0.,0.));
#11051=DIRECTION('center_axis',(0.196116135138184,-0.98058067569092,-2.17732648730911E-15));
#11052=DIRECTION('ref_axis',(-0.98058067569092,-0.196116135138184,0.));
#11053=DIRECTION('center_axis',(-0.980580675690919,0.196116135138188,0.));
#11054=DIRECTION('ref_axis',(-0.196116135138188,-0.980580675690919,0.));
#11055=DIRECTION('center_axis',(0.,0.,-1.));
#11056=DIRECTION('ref_axis',(-2.77555756156289E-15,-1.,0.));
#11057=DIRECTION('center_axis',(0.980580675690919,0.19611613513819,0.));
#11058=DIRECTION('ref_axis',(0.19611613513819,-0.980580675690919,0.));
#11059=DIRECTION('center_axis',(-0.196116135138188,-0.980580675690919,0.));
#11060=DIRECTION('ref_axis',(0.980580675690919,-0.196116135138188,0.));
#11061=DIRECTION('center_axis',(0.,0.,-1.));
#11062=DIRECTION('ref_axis',(1.,0.,0.));
#11063=DIRECTION('center_axis',(-0.196116135138184,0.98058067569092,0.));
#11064=DIRECTION('ref_axis',(0.98058067569092,0.196116135138184,0.));
#11065=DIRECTION('center_axis',(0.98058067569092,-0.196116135138184,0.));
#11066=DIRECTION('ref_axis',(0.196116135138184,0.98058067569092,0.));
#11067=DIRECTION('center_axis',(0.,0.,-1.));
#11068=DIRECTION('ref_axis',(0.,1.,0.));
#11069=DIRECTION('center_axis',(1.,1.34731136305792E-16,4.69378744770455E-33));
#11070=DIRECTION('ref_axis',(0.,0.707106781186546,-0.707106781186549));
#11071=DIRECTION('',(1.,1.34731136305792E-16,4.69378744770455E-33));
#11072=DIRECTION('',(-1.,-1.34731136305792E-16,-4.69378744770455E-33));
#11073=DIRECTION('center_axis',(-1.28138418515522E-15,-1.,-3.48381790312471E-17));
#11074=DIRECTION('ref_axis',(0.707106781186548,0.,-0.707106781186548));
#11075=DIRECTION('',(1.28138418515522E-15,1.,3.48381790312471E-17));
#11076=DIRECTION('',(-1.28138418515522E-15,-1.,-3.48381790312471E-17));
#11077=DIRECTION('center_axis',(-1.,-1.30278772428453E-49,-4.53867519783356E-66));
#11078=DIRECTION('ref_axis',(0.,-0.707106781186549,-0.707106781186546));
#11079=DIRECTION('',(1.,1.30278772428453E-49,4.53867519783356E-66));
#11080=DIRECTION('',(-1.,-1.30278772428453E-49,-4.53867519783356E-66));
#11081=DIRECTION('center_axis',(0.,1.,3.48381790312471E-17));
#11082=DIRECTION('ref_axis',(-0.707106781186548,0.,-0.707106781186548));
#11083=DIRECTION('',(0.,-1.,-3.48381790312471E-17));
#11084=DIRECTION('',(0.,1.,3.48381790312471E-17));
#11085=DIRECTION('center_axis',(1.30278772428453E-49,-1.,0.));
#11086=DIRECTION('ref_axis',(-1.,-1.30278772428453E-49,3.73954024151503E-33));
#11087=DIRECTION('',(0.,0.,-1.));
#11088=DIRECTION('',(-1.,-1.30278772428453E-49,-4.53867519783356E-66));
#11089=DIRECTION('',(0.,0.,-1.));
#11090=DIRECTION('center_axis',(0.,0.,-1.));
#11091=DIRECTION('ref_axis',(1.,5.55111512312582E-15,0.));
#11092=DIRECTION('',(0.,0.,-1.));
#11093=DIRECTION('center_axis',(0.,3.48381790312471E-17,-1.));
#11094=DIRECTION('ref_axis',(1.,5.55111512312582E-15,0.));
#11095=DIRECTION('center_axis',(1.,-1.28138418515522E-15,0.));
#11096=DIRECTION('ref_axis',(-1.28138418515522E-15,-1.,-3.48381790312471E-17));
#11097=DIRECTION('',(0.,0.,-1.));
#11098=DIRECTION('',(-1.28138418515522E-15,-1.,-3.48381790312471E-17));
#11099=DIRECTION('center_axis',(0.,0.,-1.));
#11100=DIRECTION('ref_axis',(-8.32667268468867E-15,1.,0.));
#11101=DIRECTION('',(0.,0.,-1.));
#11102=DIRECTION('center_axis',(0.,3.48381790312471E-17,-1.));
#11103=DIRECTION('ref_axis',(-8.32667268468867E-15,1.,0.));
#11104=DIRECTION('center_axis',(0.,3.48381790312471E-17,-1.));
#11105=DIRECTION('ref_axis',(-1.,0.,0.));
#11106=DIRECTION('center_axis',(0.,-3.48381790312471E-17,1.));
#11107=DIRECTION('ref_axis',(-1.,0.,0.));
#11108=DIRECTION('center_axis',(0.,-3.48381790312471E-17,1.));
#11109=DIRECTION('ref_axis',(-1.,0.,0.));
#11110=DIRECTION('center_axis',(0.,-3.48381790312471E-17,1.));
#11111=DIRECTION('ref_axis',(-1.,0.,0.));
#11112=DIRECTION('center_axis',(0.,-3.48381790312471E-17,1.));
#11113=DIRECTION('ref_axis',(-1.,0.,0.));
#11114=DIRECTION('center_axis',(-1.34731136305792E-16,1.,0.));
#11115=DIRECTION('ref_axis',(-1.,-1.34731136305792E-16,-4.69378744770455E-33));
#11116=DIRECTION('',(-1.,-1.34731136305792E-16,-4.69378744770455E-33));
#11117=DIRECTION('',(0.,0.,1.));
#11118=DIRECTION('',(-1.,-1.34731136305792E-16,-4.69378744770455E-33));
#11119=DIRECTION('',(0.,0.,1.));
#11120=DIRECTION('center_axis',(0.,0.,1.));
#11121=DIRECTION('ref_axis',(-1.,0.,0.));
#11122=DIRECTION('center_axis',(0.,-3.48381790312471E-17,1.));
#11123=DIRECTION('ref_axis',(-1.,0.,0.));
#11124=DIRECTION('',(0.,0.,1.));
#11125=DIRECTION('center_axis',(0.,-3.48381790312471E-17,1.));
#11126=DIRECTION('ref_axis',(-1.,0.,0.));
#11127=DIRECTION('center_axis',(-1.,0.,0.));
#11128=DIRECTION('ref_axis',(0.,-1.,-3.48381790312471E-17));
#11129=DIRECTION('',(0.,-1.,-3.48381790312471E-17));
#11130=DIRECTION('',(0.,0.,1.));
#11131=DIRECTION('',(0.,-1.,-3.48381790312471E-17));
#11132=DIRECTION('center_axis',(0.,0.,1.));
#11133=DIRECTION('ref_axis',(1.66533453693773E-15,-1.,0.));
#11134=DIRECTION('center_axis',(0.,-3.48381790312471E-17,1.));
#11135=DIRECTION('ref_axis',(1.66533453693773E-15,-1.,0.));
#11136=DIRECTION('',(0.,0.,1.));
#11137=DIRECTION('center_axis',(0.,-3.48381790312471E-17,1.));
#11138=DIRECTION('ref_axis',(1.66533453693773E-15,-1.,-3.48381790312471E-17));
#11139=DIRECTION('center_axis',(0.,0.,1.));
#11140=DIRECTION('ref_axis',(-5.55111512312578E-16,1.,0.));
#11141=DIRECTION('center_axis',(0.,-3.48381790312471E-17,1.));
#11142=DIRECTION('ref_axis',(-5.55111512312578E-16,1.,0.));
#11143=DIRECTION('center_axis',(0.,-3.48381790312471E-17,1.));
#11144=DIRECTION('ref_axis',(-5.55111512312578E-16,1.,3.48381790312471E-17));
#11145=DIRECTION('',(0.,0.,1.));
#11146=DIRECTION('center_axis',(1.,-6.40692092577611E-16,0.));
#11147=DIRECTION('ref_axis',(6.40692092577611E-16,1.,3.48381790312471E-17));
#11148=DIRECTION('',(6.40692092577611E-16,1.,3.48381790312471E-17));
#11149=DIRECTION('',(6.40692092577611E-16,1.,3.48381790312471E-17));
#11150=DIRECTION('',(0.,0.,1.));
#11151=DIRECTION('center_axis',(0.,0.,1.));
#11152=DIRECTION('ref_axis',(1.,1.11022302462516E-15,0.));
#11153=DIRECTION('center_axis',(0.,-3.48381790312471E-17,1.));
#11154=DIRECTION('ref_axis',(1.,1.11022302462516E-15,0.));
#11155=DIRECTION('center_axis',(0.,-3.48381790312471E-17,1.));
#11156=DIRECTION('ref_axis',(1.,1.11022302462516E-15,3.86781484965038E-32));
#11157=DIRECTION('',(0.,0.,1.));
#11158=DIRECTION('center_axis',(6.73655681528963E-17,-1.,0.));
#11159=DIRECTION('ref_axis',(1.,6.73655681528963E-17,-1.39264651766275E-33));
#11160=DIRECTION('',(1.,6.73655681528963E-17,2.34689372385228E-33));
#11161=DIRECTION('',(1.,6.73655681528963E-17,-1.39264651766275E-33));
#11162=DIRECTION('center_axis',(0.,3.48381790312471E-17,-1.));
#11163=DIRECTION('ref_axis',(-1.,0.,0.));
#11164=DIRECTION('center_axis',(0.,3.48381790312471E-17,-1.));
#11165=DIRECTION('ref_axis',(-1.,0.,0.));
#11166=DIRECTION('center_axis',(0.,3.48381790312471E-17,-1.));
#11167=DIRECTION('ref_axis',(-1.,0.,0.));
#11168=DIRECTION('center_axis',(0.,3.48381790312471E-17,-1.));
#11169=DIRECTION('ref_axis',(-1.,0.,0.));
#11170=DIRECTION('center_axis',(0.,3.48381790312471E-17,-1.));
#11171=DIRECTION('ref_axis',(-1.,0.,0.));
#11172=DIRECTION('center_axis',(0.,3.48381790312471E-17,-1.));
#11173=DIRECTION('ref_axis',(-1.,0.,0.));
#11174=DIRECTION('',(0.,1.,3.48381790312471E-17));
#11175=DIRECTION('center_axis',(0.,3.48381790312471E-17,-1.));
#11176=DIRECTION('ref_axis',(2.77555756156289E-15,-1.,0.));
#11177=DIRECTION('',(1.,1.34731136305792E-16,4.69378744770455E-33));
#11178=DIRECTION('center_axis',(0.,3.48381790312471E-17,-1.));
#11179=DIRECTION('ref_axis',(-1.,0.,0.));
#11180=DIRECTION('center_axis',(0.,0.,-1.));
#11181=DIRECTION('ref_axis',(1.,1.22464679914735E-16,0.));
#11182=DIRECTION('',(0.,0.,1.));
#11183=DIRECTION('',(0.,0.,-1.));
#11184=DIRECTION('center_axis',(0.,0.,-1.));
#11185=DIRECTION('ref_axis',(-1.,0.,0.));
#11186=DIRECTION('',(0.,0.,-1.));
#11187=DIRECTION('center_axis',(0.,0.,-1.));
#11188=DIRECTION('ref_axis',(-1.,0.,0.));
#11189=DIRECTION('',(0.,0.,-1.));
#11190=DIRECTION('center_axis',(0.,0.,-1.));
#11191=DIRECTION('ref_axis',(-1.,0.,0.));
#11192=DIRECTION('center_axis',(-1.,0.,0.));
#11193=DIRECTION('ref_axis',(0.,1.,3.48381790312471E-17));
#11194=DIRECTION('',(0.,0.,-1.));
#11195=DIRECTION('',(0.,0.,-1.));
#11196=DIRECTION('center_axis',(0.,0.,-1.));
#11197=DIRECTION('ref_axis',(2.77555756156289E-15,-1.,0.));
#11198=DIRECTION('center_axis',(-1.34731136305792E-16,1.,0.));
#11199=DIRECTION('ref_axis',(1.,1.34731136305792E-16,4.69378744770455E-33));
#11200=DIRECTION('',(0.,0.,-1.));
#11201=DIRECTION('center_axis',(0.,0.,-1.));
#11202=DIRECTION('ref_axis',(-1.,0.,0.));
#11203=DIRECTION('axis',(0.,0.,1.));
#11204=DIRECTION('refdir',(1.,0.,0.));
#11205=DIRECTION('center_axis',(0.,0.,-1.));
#11206=DIRECTION('ref_axis',(0.707106781186864,-0.707106781186231,0.));
#11207=DIRECTION('',(0.,0.,1.));
#11208=DIRECTION('center_axis',(-0.866025403784439,2.42308806056559E-16,
-0.5));
#11209=DIRECTION('ref_axis',(0.5,-1.39897054514259E-16,-0.866025403784439));
#11210=DIRECTION('center_axis',(0.,0.,-1.));
#11211=DIRECTION('ref_axis',(0.707106781186864,-0.707106781186231,0.));
#11212=DIRECTION('center_axis',(-1.34432925600244E-12,0.866025403784439,
-0.5));
#11213=DIRECTION('ref_axis',(7.76183832708735E-13,-0.5,-0.866025403784439));
#11214=DIRECTION('',(0.,0.,-1.));
#11215=DIRECTION('center_axis',(-1.,-8.96558844583498E-13,0.));
#11216=DIRECTION('ref_axis',(-8.96558844583498E-13,1.,0.));
#11217=DIRECTION('center_axis',(-1.,-8.96558844583498E-13,0.));
#11218=DIRECTION('ref_axis',(0.,0.,-1.));
#11219=DIRECTION('',(-4.48279422291749E-13,0.5,0.866025403784439));
#11220=DIRECTION('center_axis',(-1.34432925600244E-12,0.866025403784439,
-0.5));
#11221=DIRECTION('ref_axis',(1.,1.55229771566499E-12,0.));
#11222=DIRECTION('center_axis',(-1.34432925600244E-12,0.866025403784439,
-0.5));
#11223=DIRECTION('ref_axis',(0.,-0.5,-0.866025403784439));
#11224=DIRECTION('',(-1.,-1.55229771566499E-12,0.));
#11225=DIRECTION('center_axis',(-1.34432925600244E-12,0.866025403784439,
-0.5));
#11226=DIRECTION('ref_axis',(7.76183832708735E-13,-0.5,-0.866025403784439));
#11227=DIRECTION('',(7.28095205575773E-14,-0.5,-0.866025403784439));
#11228=DIRECTION('center_axis',(1.,1.45619041115155E-13,0.));
#11229=DIRECTION('ref_axis',(1.45619041115155E-13,-1.,0.));
#11230=DIRECTION('center_axis',(1.,1.45619041115155E-13,0.));
#11231=DIRECTION('ref_axis',(0.,0.,1.));
#11232=DIRECTION('',(0.,0.,1.));
#11233=DIRECTION('center_axis',(0.,0.,-1.));
#11234=DIRECTION('ref_axis',(-0.707106781186035,-0.70710678118706,0.));
#11235=DIRECTION('center_axis',(0.,0.,-1.));
#11236=DIRECTION('ref_axis',(-0.707106781186035,-0.70710678118706,0.));
#11237=DIRECTION('center_axis',(0.866025403784439,1.82700839766916E-13,
-0.5));
#11238=DIRECTION('ref_axis',(-0.5,-1.0551735336738E-13,-0.866025403784439));
#11239=DIRECTION('',(0.,0.,-1.));
#11240=DIRECTION('center_axis',(-1.30466679482154E-12,1.,0.));
#11241=DIRECTION('ref_axis',(1.,1.30466679482154E-12,0.));
#11242=DIRECTION('center_axis',(-1.30466679482154E-12,1.,0.));
#11243=DIRECTION('ref_axis',(0.,0.,-1.));
#11244=DIRECTION('',(0.5,6.52333397410772E-13,0.866025403784439));
#11245=DIRECTION('center_axis',(0.866025403784439,1.82700839766916E-13,
-0.5));
#11246=DIRECTION('ref_axis',(2.10964758041199E-13,-1.,0.));
#11247=DIRECTION('center_axis',(0.866025403784439,1.82700839766916E-13,
-0.5));
#11248=DIRECTION('ref_axis',(0.5,0.,0.866025403784439));
#11249=DIRECTION('',(-2.10964758041199E-13,1.,0.));
#11250=DIRECTION('center_axis',(0.866025403784439,1.82700839766916E-13,
-0.5));
#11251=DIRECTION('ref_axis',(-0.5,-1.05482379103751E-13,-0.866025403784439));
#11252=DIRECTION('',(-0.5,6.4832235838889E-13,-0.866025403784439));
#11253=DIRECTION('center_axis',(-1.29664471677778E-12,-1.,0.));
#11254=DIRECTION('ref_axis',(-1.,1.29664471677778E-12,0.));
#11255=DIRECTION('center_axis',(-1.29664471677778E-12,-1.,0.));
#11256=DIRECTION('ref_axis',(0.,0.,1.));
#11257=DIRECTION('',(0.,0.,1.));
#11258=DIRECTION('center_axis',(0.,0.,-1.));
#11259=DIRECTION('ref_axis',(0.707106781186895,0.7071067811862,0.));
#11260=DIRECTION('',(0.,0.,1.));
#11261=DIRECTION('center_axis',(-1.35644469630397E-12,-0.866025403784439,
-0.5));
#11262=DIRECTION('ref_axis',(7.8314371117082E-13,0.5,-0.866025403784439));
#11263=DIRECTION('center_axis',(0.,0.,-1.));
#11264=DIRECTION('ref_axis',(0.707106781186895,0.7071067811862,0.));
#11265=DIRECTION('center_axis',(-0.866025403784439,2.42308806056559E-16,
-0.5));
#11266=DIRECTION('ref_axis',(0.5,-1.39897054514259E-16,-0.866025403784439));
#11267=DIRECTION('',(0.,0.,-1.));
#11268=DIRECTION('center_axis',(1.80920256647203E-12,-1.,0.));
#11269=DIRECTION('ref_axis',(-1.,-1.80920256647203E-12,0.));
#11270=DIRECTION('center_axis',(1.80920256647203E-12,-1.,0.));
#11271=DIRECTION('ref_axis',(0.,0.,1.));
#11272=DIRECTION('',(-0.5,-9.04601283236015E-13,0.866025403784439));
#11273=DIRECTION('center_axis',(0.,0.,-1.));
#11274=DIRECTION('ref_axis',(-0.707106781186768,0.707106781186327,0.));
#11275=DIRECTION('center_axis',(0.,0.,-1.));
#11276=DIRECTION('ref_axis',(-0.707106781186768,0.707106781186327,0.));
#11277=DIRECTION('center_axis',(-1.35644469630397E-12,-0.866025403784439,
-0.5));
#11278=DIRECTION('ref_axis',(7.83108736907191E-13,0.5,-0.866025403784439));
#11279=DIRECTION('',(0.,0.,-1.));
#11280=DIRECTION('center_axis',(1.,1.91935343509834E-12,0.));
#11281=DIRECTION('ref_axis',(1.91935343509834E-12,-1.,0.));
#11282=DIRECTION('center_axis',(1.,1.91935343509834E-12,0.));
#11283=DIRECTION('ref_axis',(0.,0.,1.));
#11284=DIRECTION('',(9.59676717549172E-13,-0.5,0.866025403784439));
#11285=DIRECTION('center_axis',(-1.62884833462111E-16,1.,0.));
#11286=DIRECTION('ref_axis',(1.,1.62884833462111E-16,0.));
#11287=DIRECTION('center_axis',(-1.62884833462111E-16,1.,0.));
#11288=DIRECTION('ref_axis',(0.,0.,-1.));
#11289=DIRECTION('',(0.5,8.14424167310554E-17,-0.866025403784439));
#11290=DIRECTION('center_axis',(-0.866025403784439,2.42308806056559E-16,
-0.5));
#11291=DIRECTION('ref_axis',(2.79794108807543E-16,1.,0.));
#11292=DIRECTION('center_axis',(-0.866025403784439,2.42308806056559E-16,
-0.5));
#11293=DIRECTION('ref_axis',(0.5,0.,-0.866025403784439));
#11294=DIRECTION('',(-2.79794108807543E-16,-1.,0.));
#11295=DIRECTION('center_axis',(-0.866025403784439,2.42308806056559E-16,
-0.5));
#11296=DIRECTION('ref_axis',(0.5,0.,-0.866025403784439));
#11297=DIRECTION('center_axis',(-1.,2.79168316070879E-12,0.));
#11298=DIRECTION('ref_axis',(2.79168316070879E-12,1.,0.));
#11299=DIRECTION('center_axis',(-1.,2.79168316070879E-12,0.));
#11300=DIRECTION('ref_axis',(0.,0.,-1.));
#11301=DIRECTION('',(1.3958415803544E-12,0.5,-0.866025403784439));
#11302=DIRECTION('center_axis',(-1.35644469630397E-12,-0.866025403784439,
-0.5));
#11303=DIRECTION('ref_axis',(-1.,1.56628742110387E-12,0.));
#11304=DIRECTION('center_axis',(-1.35644469630397E-12,-0.866025403784439,
-0.5));
#11305=DIRECTION('ref_axis',(0.,-0.5,0.866025403784439));
#11306=DIRECTION('',(1.,-1.56628742110387E-12,0.));
#11307=DIRECTION('center_axis',(0.,0.,-1.));
#11308=DIRECTION('ref_axis',(-1.,0.,0.));
#11309=DIRECTION('center_axis',(0.,0.,-1.));
#11310=DIRECTION('ref_axis',(-1.,0.,0.));
#11311=DIRECTION('center_axis',(0.,0.,-1.));
#11312=DIRECTION('ref_axis',(1.,0.,0.));
#11313=DIRECTION('center_axis',(-1.22464679914735E-16,-1.,0.));
#11314=DIRECTION('ref_axis',(1.,-1.22464679914735E-16,0.));
#11315=DIRECTION('center_axis',(0.,0.,1.));
#11316=DIRECTION('ref_axis',(1.,0.,0.));
#11317=DIRECTION('center_axis',(0.,0.,-1.));
#11318=DIRECTION('ref_axis',(-1.,0.,0.));
#11319=DIRECTION('center_axis',(0.,0.,-1.));
#11320=DIRECTION('ref_axis',(1.,0.,0.));
#11321=DIRECTION('center_axis',(0.,0.,-1.));
#11322=DIRECTION('ref_axis',(-1.,0.,0.));
#11323=DIRECTION('center_axis',(0.,0.,-1.));
#11324=DIRECTION('ref_axis',(1.,0.,0.));
#11325=DIRECTION('',(0.,0.,1.));
#11326=DIRECTION('center_axis',(0.,0.,-1.));
#11327=DIRECTION('ref_axis',(-1.,0.,0.));
#11328=DIRECTION('center_axis',(0.,0.,-1.));
#11329=DIRECTION('ref_axis',(-1.,0.,0.));
#11330=DIRECTION('',(-0.258819045102519,3.16961915143174E-17,0.965925826289069));
#11331=DIRECTION('center_axis',(0.,0.,-1.));
#11332=DIRECTION('ref_axis',(-1.,0.,0.));
#11333=DIRECTION('center_axis',(0.,0.,1.));
#11334=DIRECTION('ref_axis',(-1.,0.,0.));
#11335=DIRECTION('',(0.,0.,1.));
#11336=DIRECTION('center_axis',(0.,0.,-1.));
#11337=DIRECTION('ref_axis',(-1.,0.,0.));
#11338=DIRECTION('center_axis',(6.12323399573676E-17,0.,1.));
#11339=DIRECTION('ref_axis',(1.,0.,0.));
#11340=DIRECTION('center_axis',(1.22464679914735E-16,-1.,0.));
#11341=DIRECTION('ref_axis',(-1.,-1.22464679914735E-16,0.));
#11342=DIRECTION('center_axis',(0.,0.,-1.));
#11343=DIRECTION('ref_axis',(1.,0.,0.));
#11344=DIRECTION('center_axis',(0.,0.,-1.));
#11345=DIRECTION('ref_axis',(1.,0.,0.));
#11346=DIRECTION('center_axis',(0.,0.,-1.));
#11347=DIRECTION('ref_axis',(-1.,0.,0.));
#11348=DIRECTION('',(-0.087155742757872,1.06735001395738E-17,0.996194698090852));
#11349=DIRECTION('axis',(0.,0.,1.));
#11350=DIRECTION('refdir',(1.,0.,0.));
#11351=DIRECTION('center_axis',(0.,0.,-1.));
#11352=DIRECTION('ref_axis',(0.707106781186864,-0.707106781186231,0.));
#11353=DIRECTION('',(0.,0.,1.));
#11354=DIRECTION('center_axis',(-0.866025403784439,2.42308806056559E-16,
-0.5));
#11355=DIRECTION('ref_axis',(0.5,-1.39897054514259E-16,-0.866025403784439));
#11356=DIRECTION('center_axis',(0.,0.,-1.));
#11357=DIRECTION('ref_axis',(0.707106781186864,-0.707106781186231,0.));
#11358=DIRECTION('center_axis',(-1.34432925600244E-12,0.866025403784439,
-0.5));
#11359=DIRECTION('ref_axis',(7.76183832708735E-13,-0.5,-0.866025403784439));
#11360=DIRECTION('',(0.,0.,-1.));
#11361=DIRECTION('center_axis',(-1.,-8.96558844583498E-13,0.));
#11362=DIRECTION('ref_axis',(-8.96558844583498E-13,1.,0.));
#11363=DIRECTION('center_axis',(-1.,-8.96558844583498E-13,0.));
#11364=DIRECTION('ref_axis',(0.,0.,-1.));
#11365=DIRECTION('',(-4.48279422291749E-13,0.5,0.866025403784439));
#11366=DIRECTION('center_axis',(-1.34432925600244E-12,0.866025403784439,
-0.5));
#11367=DIRECTION('ref_axis',(1.,1.55229771566499E-12,0.));
#11368=DIRECTION('center_axis',(-1.34432925600244E-12,0.866025403784439,
-0.5));
#11369=DIRECTION('ref_axis',(0.,-0.5,-0.866025403784439));
#11370=DIRECTION('',(-1.,-1.55229771566499E-12,0.));
#11371=DIRECTION('center_axis',(-1.34432925600244E-12,0.866025403784439,
-0.5));
#11372=DIRECTION('ref_axis',(7.76183832708735E-13,-0.5,-0.866025403784439));
#11373=DIRECTION('',(7.28095205575773E-14,-0.5,-0.866025403784439));
#11374=DIRECTION('center_axis',(1.,1.45619041115155E-13,0.));
#11375=DIRECTION('ref_axis',(1.45619041115155E-13,-1.,0.));
#11376=DIRECTION('center_axis',(1.,1.45619041115155E-13,0.));
#11377=DIRECTION('ref_axis',(0.,0.,1.));
#11378=DIRECTION('',(0.,0.,1.));
#11379=DIRECTION('center_axis',(0.,0.,-1.));
#11380=DIRECTION('ref_axis',(-0.707106781186035,-0.70710678118706,0.));
#11381=DIRECTION('center_axis',(0.,0.,-1.));
#11382=DIRECTION('ref_axis',(-0.707106781186035,-0.70710678118706,0.));
#11383=DIRECTION('center_axis',(0.866025403784439,1.82700839766916E-13,
-0.5));
#11384=DIRECTION('ref_axis',(-0.5,-1.0551735336738E-13,-0.866025403784439));
#11385=DIRECTION('',(0.,0.,-1.));
#11386=DIRECTION('center_axis',(-1.30466679482154E-12,1.,0.));
#11387=DIRECTION('ref_axis',(1.,1.30466679482154E-12,0.));
#11388=DIRECTION('center_axis',(-1.30466679482154E-12,1.,0.));
#11389=DIRECTION('ref_axis',(0.,0.,-1.));
#11390=DIRECTION('',(0.5,6.52333397410772E-13,0.866025403784439));
#11391=DIRECTION('center_axis',(0.866025403784439,1.82700839766916E-13,
-0.5));
#11392=DIRECTION('ref_axis',(2.10964758041199E-13,-1.,0.));
#11393=DIRECTION('center_axis',(0.866025403784439,1.82700839766916E-13,
-0.5));
#11394=DIRECTION('ref_axis',(0.5,0.,0.866025403784439));
#11395=DIRECTION('',(-2.10964758041199E-13,1.,0.));
#11396=DIRECTION('center_axis',(0.866025403784439,1.82700839766916E-13,
-0.5));
#11397=DIRECTION('ref_axis',(-0.5,-1.05482379103751E-13,-0.866025403784439));
#11398=DIRECTION('',(-0.5,6.4832235838889E-13,-0.866025403784439));
#11399=DIRECTION('center_axis',(-1.29664471677778E-12,-1.,0.));
#11400=DIRECTION('ref_axis',(-1.,1.29664471677778E-12,0.));
#11401=DIRECTION('center_axis',(-1.29664471677778E-12,-1.,0.));
#11402=DIRECTION('ref_axis',(0.,0.,1.));
#11403=DIRECTION('',(0.,0.,1.));
#11404=DIRECTION('center_axis',(0.,0.,-1.));
#11405=DIRECTION('ref_axis',(0.707106781186895,0.7071067811862,0.));
#11406=DIRECTION('',(0.,0.,1.));
#11407=DIRECTION('center_axis',(-1.35644469630397E-12,-0.866025403784439,
-0.5));
#11408=DIRECTION('ref_axis',(7.8314371117082E-13,0.5,-0.866025403784439));
#11409=DIRECTION('center_axis',(0.,0.,-1.));
#11410=DIRECTION('ref_axis',(0.707106781186895,0.7071067811862,0.));
#11411=DIRECTION('center_axis',(-0.866025403784439,2.42308806056559E-16,
-0.5));
#11412=DIRECTION('ref_axis',(0.5,-1.39897054514259E-16,-0.866025403784439));
#11413=DIRECTION('',(0.,0.,-1.));
#11414=DIRECTION('center_axis',(1.80920256647203E-12,-1.,0.));
#11415=DIRECTION('ref_axis',(-1.,-1.80920256647203E-12,0.));
#11416=DIRECTION('center_axis',(1.80920256647203E-12,-1.,0.));
#11417=DIRECTION('ref_axis',(0.,0.,1.));
#11418=DIRECTION('',(-0.5,-9.04601283236015E-13,0.866025403784439));
#11419=DIRECTION('center_axis',(0.,0.,-1.));
#11420=DIRECTION('ref_axis',(-0.707106781186768,0.707106781186327,0.));
#11421=DIRECTION('center_axis',(0.,0.,-1.));
#11422=DIRECTION('ref_axis',(-0.707106781186768,0.707106781186327,0.));
#11423=DIRECTION('center_axis',(-1.35644469630397E-12,-0.866025403784439,
-0.5));
#11424=DIRECTION('ref_axis',(7.83108736907191E-13,0.5,-0.866025403784439));
#11425=DIRECTION('',(0.,0.,-1.));
#11426=DIRECTION('center_axis',(1.,1.91935343509834E-12,0.));
#11427=DIRECTION('ref_axis',(1.91935343509834E-12,-1.,0.));
#11428=DIRECTION('center_axis',(1.,1.91935343509834E-12,0.));
#11429=DIRECTION('ref_axis',(0.,0.,1.));
#11430=DIRECTION('',(9.59676717549172E-13,-0.5,0.866025403784439));
#11431=DIRECTION('center_axis',(-1.62884833462111E-16,1.,0.));
#11432=DIRECTION('ref_axis',(1.,1.62884833462111E-16,0.));
#11433=DIRECTION('center_axis',(-1.62884833462111E-16,1.,0.));
#11434=DIRECTION('ref_axis',(0.,0.,-1.));
#11435=DIRECTION('',(0.5,8.14424167310554E-17,-0.866025403784439));
#11436=DIRECTION('center_axis',(-0.866025403784439,2.42308806056559E-16,
-0.5));
#11437=DIRECTION('ref_axis',(2.79794108807543E-16,1.,0.));
#11438=DIRECTION('center_axis',(-0.866025403784439,2.42308806056559E-16,
-0.5));
#11439=DIRECTION('ref_axis',(0.5,0.,-0.866025403784439));
#11440=DIRECTION('',(-2.79794108807543E-16,-1.,0.));
#11441=DIRECTION('center_axis',(-0.866025403784439,2.42308806056559E-16,
-0.5));
#11442=DIRECTION('ref_axis',(0.5,0.,-0.866025403784439));
#11443=DIRECTION('center_axis',(-1.,2.79168316070879E-12,0.));
#11444=DIRECTION('ref_axis',(2.79168316070879E-12,1.,0.));
#11445=DIRECTION('center_axis',(-1.,2.79168316070879E-12,0.));
#11446=DIRECTION('ref_axis',(0.,0.,-1.));
#11447=DIRECTION('',(1.3958415803544E-12,0.5,-0.866025403784439));
#11448=DIRECTION('center_axis',(-1.35644469630397E-12,-0.866025403784439,
-0.5));
#11449=DIRECTION('ref_axis',(-1.,1.56628742110387E-12,0.));
#11450=DIRECTION('center_axis',(-1.35644469630397E-12,-0.866025403784439,
-0.5));
#11451=DIRECTION('ref_axis',(0.,-0.5,0.866025403784439));
#11452=DIRECTION('',(1.,-1.56628742110387E-12,0.));
#11453=DIRECTION('center_axis',(0.,0.,-1.));
#11454=DIRECTION('ref_axis',(-1.,0.,0.));
#11455=DIRECTION('center_axis',(0.,0.,-1.));
#11456=DIRECTION('ref_axis',(-1.,0.,0.));
#11457=DIRECTION('center_axis',(0.,0.,-1.));
#11458=DIRECTION('ref_axis',(1.,0.,0.));
#11459=DIRECTION('center_axis',(-1.22464679914735E-16,-1.,0.));
#11460=DIRECTION('ref_axis',(1.,-1.22464679914735E-16,0.));
#11461=DIRECTION('center_axis',(0.,0.,1.));
#11462=DIRECTION('ref_axis',(1.,0.,0.));
#11463=DIRECTION('center_axis',(0.,0.,-1.));
#11464=DIRECTION('ref_axis',(-1.,0.,0.));
#11465=DIRECTION('center_axis',(0.,0.,-1.));
#11466=DIRECTION('ref_axis',(1.,0.,0.));
#11467=DIRECTION('center_axis',(0.,0.,-1.));
#11468=DIRECTION('ref_axis',(-1.,0.,0.));
#11469=DIRECTION('center_axis',(0.,0.,-1.));
#11470=DIRECTION('ref_axis',(1.,0.,0.));
#11471=DIRECTION('',(0.,0.,1.));
#11472=DIRECTION('center_axis',(0.,0.,-1.));
#11473=DIRECTION('ref_axis',(-1.,0.,0.));
#11474=DIRECTION('center_axis',(0.,0.,-1.));
#11475=DIRECTION('ref_axis',(-1.,0.,0.));
#11476=DIRECTION('',(-0.258819045102519,3.16961915143174E-17,0.965925826289069));
#11477=DIRECTION('center_axis',(0.,0.,-1.));
#11478=DIRECTION('ref_axis',(-1.,0.,0.));
#11479=DIRECTION('center_axis',(0.,0.,1.));
#11480=DIRECTION('ref_axis',(-1.,0.,0.));
#11481=DIRECTION('',(0.,0.,1.));
#11482=DIRECTION('center_axis',(0.,0.,-1.));
#11483=DIRECTION('ref_axis',(-1.,0.,0.));
#11484=DIRECTION('center_axis',(6.12323399573676E-17,0.,1.));
#11485=DIRECTION('ref_axis',(1.,0.,0.));
#11486=DIRECTION('center_axis',(1.22464679914735E-16,-1.,0.));
#11487=DIRECTION('ref_axis',(-1.,-1.22464679914735E-16,0.));
#11488=DIRECTION('center_axis',(0.,0.,-1.));
#11489=DIRECTION('ref_axis',(1.,0.,0.));
#11490=DIRECTION('center_axis',(0.,0.,-1.));
#11491=DIRECTION('ref_axis',(1.,0.,0.));
#11492=DIRECTION('center_axis',(0.,0.,-1.));
#11493=DIRECTION('ref_axis',(-1.,0.,0.));
#11494=DIRECTION('',(-0.087155742757872,1.06735001395738E-17,0.996194698090852));
#11495=DIRECTION('axis',(0.,0.,1.));
#11496=DIRECTION('refdir',(1.,0.,0.));
#11497=DIRECTION('center_axis',(0.,0.,-1.));
#11498=DIRECTION('ref_axis',(0.707106781186864,-0.707106781186231,0.));
#11499=DIRECTION('',(0.,0.,1.));
#11500=DIRECTION('center_axis',(-0.866025403784439,2.42308806056559E-16,
-0.5));
#11501=DIRECTION('ref_axis',(0.5,-1.39897054514259E-16,-0.866025403784439));
#11502=DIRECTION('center_axis',(0.,0.,-1.));
#11503=DIRECTION('ref_axis',(0.707106781186864,-0.707106781186231,0.));
#11504=DIRECTION('center_axis',(-1.34432925600244E-12,0.866025403784439,
-0.5));
#11505=DIRECTION('ref_axis',(7.76183832708735E-13,-0.5,-0.866025403784439));
#11506=DIRECTION('',(0.,0.,-1.));
#11507=DIRECTION('center_axis',(-1.,-8.96558844583498E-13,0.));
#11508=DIRECTION('ref_axis',(-8.96558844583498E-13,1.,0.));
#11509=DIRECTION('center_axis',(-1.,-8.96558844583498E-13,0.));
#11510=DIRECTION('ref_axis',(0.,0.,-1.));
#11511=DIRECTION('',(-4.48279422291749E-13,0.5,0.866025403784439));
#11512=DIRECTION('center_axis',(-1.34432925600244E-12,0.866025403784439,
-0.5));
#11513=DIRECTION('ref_axis',(1.,1.55229771566499E-12,0.));
#11514=DIRECTION('center_axis',(-1.34432925600244E-12,0.866025403784439,
-0.5));
#11515=DIRECTION('ref_axis',(0.,-0.5,-0.866025403784439));
#11516=DIRECTION('',(-1.,-1.55229771566499E-12,0.));
#11517=DIRECTION('center_axis',(-1.34432925600244E-12,0.866025403784439,
-0.5));
#11518=DIRECTION('ref_axis',(7.76183832708735E-13,-0.5,-0.866025403784439));
#11519=DIRECTION('',(7.28095205575773E-14,-0.5,-0.866025403784439));
#11520=DIRECTION('center_axis',(1.,1.45619041115155E-13,0.));
#11521=DIRECTION('ref_axis',(1.45619041115155E-13,-1.,0.));
#11522=DIRECTION('center_axis',(1.,1.45619041115155E-13,0.));
#11523=DIRECTION('ref_axis',(0.,0.,1.));
#11524=DIRECTION('',(0.,0.,1.));
#11525=DIRECTION('center_axis',(0.,0.,-1.));
#11526=DIRECTION('ref_axis',(-0.707106781186035,-0.70710678118706,0.));
#11527=DIRECTION('center_axis',(0.,0.,-1.));
#11528=DIRECTION('ref_axis',(-0.707106781186035,-0.70710678118706,0.));
#11529=DIRECTION('center_axis',(0.866025403784439,1.82700839766916E-13,
-0.5));
#11530=DIRECTION('ref_axis',(-0.5,-1.0551735336738E-13,-0.866025403784439));
#11531=DIRECTION('',(0.,0.,-1.));
#11532=DIRECTION('center_axis',(-1.30466679482154E-12,1.,0.));
#11533=DIRECTION('ref_axis',(1.,1.30466679482154E-12,0.));
#11534=DIRECTION('center_axis',(-1.30466679482154E-12,1.,0.));
#11535=DIRECTION('ref_axis',(0.,0.,-1.));
#11536=DIRECTION('',(0.5,6.52333397410772E-13,0.866025403784439));
#11537=DIRECTION('center_axis',(0.866025403784439,1.82700839766916E-13,
-0.5));
#11538=DIRECTION('ref_axis',(2.10964758041199E-13,-1.,0.));
#11539=DIRECTION('center_axis',(0.866025403784439,1.82700839766916E-13,
-0.5));
#11540=DIRECTION('ref_axis',(0.5,0.,0.866025403784439));
#11541=DIRECTION('',(-2.10964758041199E-13,1.,0.));
#11542=DIRECTION('center_axis',(0.866025403784439,1.82700839766916E-13,
-0.5));
#11543=DIRECTION('ref_axis',(-0.5,-1.05482379103751E-13,-0.866025403784439));
#11544=DIRECTION('',(-0.5,6.4832235838889E-13,-0.866025403784439));
#11545=DIRECTION('center_axis',(-1.29664471677778E-12,-1.,0.));
#11546=DIRECTION('ref_axis',(-1.,1.29664471677778E-12,0.));
#11547=DIRECTION('center_axis',(-1.29664471677778E-12,-1.,0.));
#11548=DIRECTION('ref_axis',(0.,0.,1.));
#11549=DIRECTION('',(0.,0.,1.));
#11550=DIRECTION('center_axis',(0.,0.,-1.));
#11551=DIRECTION('ref_axis',(0.707106781186895,0.7071067811862,0.));
#11552=DIRECTION('',(0.,0.,1.));
#11553=DIRECTION('center_axis',(-1.35644469630397E-12,-0.866025403784439,
-0.5));
#11554=DIRECTION('ref_axis',(7.8314371117082E-13,0.5,-0.866025403784439));
#11555=DIRECTION('center_axis',(0.,0.,-1.));
#11556=DIRECTION('ref_axis',(0.707106781186895,0.7071067811862,0.));
#11557=DIRECTION('center_axis',(-0.866025403784439,2.42308806056559E-16,
-0.5));
#11558=DIRECTION('ref_axis',(0.5,-1.39897054514259E-16,-0.866025403784439));
#11559=DIRECTION('',(0.,0.,-1.));
#11560=DIRECTION('center_axis',(1.80920256647203E-12,-1.,0.));
#11561=DIRECTION('ref_axis',(-1.,-1.80920256647203E-12,0.));
#11562=DIRECTION('center_axis',(1.80920256647203E-12,-1.,0.));
#11563=DIRECTION('ref_axis',(0.,0.,1.));
#11564=DIRECTION('',(-0.5,-9.04601283236015E-13,0.866025403784439));
#11565=DIRECTION('center_axis',(0.,0.,-1.));
#11566=DIRECTION('ref_axis',(-0.707106781186768,0.707106781186327,0.));
#11567=DIRECTION('center_axis',(0.,0.,-1.));
#11568=DIRECTION('ref_axis',(-0.707106781186768,0.707106781186327,0.));
#11569=DIRECTION('center_axis',(-1.35644469630397E-12,-0.866025403784439,
-0.5));
#11570=DIRECTION('ref_axis',(7.83108736907191E-13,0.5,-0.866025403784439));
#11571=DIRECTION('',(0.,0.,-1.));
#11572=DIRECTION('center_axis',(1.,1.91935343509834E-12,0.));
#11573=DIRECTION('ref_axis',(1.91935343509834E-12,-1.,0.));
#11574=DIRECTION('center_axis',(1.,1.91935343509834E-12,0.));
#11575=DIRECTION('ref_axis',(0.,0.,1.));
#11576=DIRECTION('',(9.59676717549172E-13,-0.5,0.866025403784439));
#11577=DIRECTION('center_axis',(-1.62884833462111E-16,1.,0.));
#11578=DIRECTION('ref_axis',(1.,1.62884833462111E-16,0.));
#11579=DIRECTION('center_axis',(-1.62884833462111E-16,1.,0.));
#11580=DIRECTION('ref_axis',(0.,0.,-1.));
#11581=DIRECTION('',(0.5,8.14424167310554E-17,-0.866025403784439));
#11582=DIRECTION('center_axis',(-0.866025403784439,2.42308806056559E-16,
-0.5));
#11583=DIRECTION('ref_axis',(2.79794108807543E-16,1.,0.));
#11584=DIRECTION('center_axis',(-0.866025403784439,2.42308806056559E-16,
-0.5));
#11585=DIRECTION('ref_axis',(0.5,0.,-0.866025403784439));
#11586=DIRECTION('',(-2.79794108807543E-16,-1.,0.));
#11587=DIRECTION('center_axis',(-0.866025403784439,2.42308806056559E-16,
-0.5));
#11588=DIRECTION('ref_axis',(0.5,0.,-0.866025403784439));
#11589=DIRECTION('center_axis',(-1.,2.79168316070879E-12,0.));
#11590=DIRECTION('ref_axis',(2.79168316070879E-12,1.,0.));
#11591=DIRECTION('center_axis',(-1.,2.79168316070879E-12,0.));
#11592=DIRECTION('ref_axis',(0.,0.,-1.));
#11593=DIRECTION('',(1.3958415803544E-12,0.5,-0.866025403784439));
#11594=DIRECTION('center_axis',(-1.35644469630397E-12,-0.866025403784439,
-0.5));
#11595=DIRECTION('ref_axis',(-1.,1.56628742110387E-12,0.));
#11596=DIRECTION('center_axis',(-1.35644469630397E-12,-0.866025403784439,
-0.5));
#11597=DIRECTION('ref_axis',(0.,-0.5,0.866025403784439));
#11598=DIRECTION('',(1.,-1.56628742110387E-12,0.));
#11599=DIRECTION('center_axis',(0.,0.,-1.));
#11600=DIRECTION('ref_axis',(-1.,0.,0.));
#11601=DIRECTION('center_axis',(0.,0.,-1.));
#11602=DIRECTION('ref_axis',(-1.,0.,0.));
#11603=DIRECTION('center_axis',(0.,0.,-1.));
#11604=DIRECTION('ref_axis',(1.,0.,0.));
#11605=DIRECTION('center_axis',(-1.22464679914735E-16,-1.,0.));
#11606=DIRECTION('ref_axis',(1.,-1.22464679914735E-16,0.));
#11607=DIRECTION('center_axis',(0.,0.,1.));
#11608=DIRECTION('ref_axis',(1.,0.,0.));
#11609=DIRECTION('center_axis',(0.,0.,-1.));
#11610=DIRECTION('ref_axis',(-1.,0.,0.));
#11611=DIRECTION('center_axis',(0.,0.,-1.));
#11612=DIRECTION('ref_axis',(1.,0.,0.));
#11613=DIRECTION('center_axis',(0.,0.,-1.));
#11614=DIRECTION('ref_axis',(-1.,0.,0.));
#11615=DIRECTION('center_axis',(0.,0.,-1.));
#11616=DIRECTION('ref_axis',(1.,0.,0.));
#11617=DIRECTION('',(0.,0.,1.));
#11618=DIRECTION('center_axis',(0.,0.,-1.));
#11619=DIRECTION('ref_axis',(-1.,0.,0.));
#11620=DIRECTION('center_axis',(0.,0.,-1.));
#11621=DIRECTION('ref_axis',(-1.,0.,0.));
#11622=DIRECTION('',(-0.258819045102519,3.16961915143174E-17,0.965925826289069));
#11623=DIRECTION('center_axis',(0.,0.,-1.));
#11624=DIRECTION('ref_axis',(-1.,0.,0.));
#11625=DIRECTION('center_axis',(0.,0.,1.));
#11626=DIRECTION('ref_axis',(-1.,0.,0.));
#11627=DIRECTION('',(0.,0.,1.));
#11628=DIRECTION('center_axis',(0.,0.,-1.));
#11629=DIRECTION('ref_axis',(-1.,0.,0.));
#11630=DIRECTION('center_axis',(6.12323399573676E-17,0.,1.));
#11631=DIRECTION('ref_axis',(1.,0.,0.));
#11632=DIRECTION('center_axis',(1.22464679914735E-16,-1.,0.));
#11633=DIRECTION('ref_axis',(-1.,-1.22464679914735E-16,0.));
#11634=DIRECTION('center_axis',(0.,0.,-1.));
#11635=DIRECTION('ref_axis',(1.,0.,0.));
#11636=DIRECTION('center_axis',(0.,0.,-1.));
#11637=DIRECTION('ref_axis',(1.,0.,0.));
#11638=DIRECTION('center_axis',(0.,0.,-1.));
#11639=DIRECTION('ref_axis',(-1.,0.,0.));
#11640=DIRECTION('',(-0.087155742757872,1.06735001395738E-17,0.996194698090852));
#11641=DIRECTION('axis',(0.,0.,1.));
#11642=DIRECTION('refdir',(1.,0.,0.));
#11643=DIRECTION('center_axis',(0.,0.,-1.));
#11644=DIRECTION('ref_axis',(0.707106781186864,-0.707106781186231,0.));
#11645=DIRECTION('',(0.,0.,1.));
#11646=DIRECTION('center_axis',(-0.866025403784439,2.42308806056559E-16,
-0.5));
#11647=DIRECTION('ref_axis',(0.5,-1.39897054514259E-16,-0.866025403784439));
#11648=DIRECTION('center_axis',(0.,0.,-1.));
#11649=DIRECTION('ref_axis',(0.707106781186864,-0.707106781186231,0.));
#11650=DIRECTION('center_axis',(-1.34432925600244E-12,0.866025403784439,
-0.5));
#11651=DIRECTION('ref_axis',(7.76183832708735E-13,-0.5,-0.866025403784439));
#11652=DIRECTION('',(0.,0.,-1.));
#11653=DIRECTION('center_axis',(-1.,-8.96558844583498E-13,0.));
#11654=DIRECTION('ref_axis',(-8.96558844583498E-13,1.,0.));
#11655=DIRECTION('center_axis',(-1.,-8.96558844583498E-13,0.));
#11656=DIRECTION('ref_axis',(0.,0.,-1.));
#11657=DIRECTION('',(-4.48279422291749E-13,0.5,0.866025403784439));
#11658=DIRECTION('center_axis',(-1.34432925600244E-12,0.866025403784439,
-0.5));
#11659=DIRECTION('ref_axis',(1.,1.55229771566499E-12,0.));
#11660=DIRECTION('center_axis',(-1.34432925600244E-12,0.866025403784439,
-0.5));
#11661=DIRECTION('ref_axis',(0.,-0.5,-0.866025403784439));
#11662=DIRECTION('',(-1.,-1.55229771566499E-12,0.));
#11663=DIRECTION('center_axis',(-1.34432925600244E-12,0.866025403784439,
-0.5));
#11664=DIRECTION('ref_axis',(7.76183832708735E-13,-0.5,-0.866025403784439));
#11665=DIRECTION('',(7.28095205575773E-14,-0.5,-0.866025403784439));
#11666=DIRECTION('center_axis',(1.,1.45619041115155E-13,0.));
#11667=DIRECTION('ref_axis',(1.45619041115155E-13,-1.,0.));
#11668=DIRECTION('center_axis',(1.,1.45619041115155E-13,0.));
#11669=DIRECTION('ref_axis',(0.,0.,1.));
#11670=DIRECTION('',(0.,0.,1.));
#11671=DIRECTION('center_axis',(0.,0.,-1.));
#11672=DIRECTION('ref_axis',(-0.707106781186035,-0.70710678118706,0.));
#11673=DIRECTION('center_axis',(0.,0.,-1.));
#11674=DIRECTION('ref_axis',(-0.707106781186035,-0.70710678118706,0.));
#11675=DIRECTION('center_axis',(0.866025403784439,1.82700839766916E-13,
-0.5));
#11676=DIRECTION('ref_axis',(-0.5,-1.0551735336738E-13,-0.866025403784439));
#11677=DIRECTION('',(0.,0.,-1.));
#11678=DIRECTION('center_axis',(-1.30466679482154E-12,1.,0.));
#11679=DIRECTION('ref_axis',(1.,1.30466679482154E-12,0.));
#11680=DIRECTION('center_axis',(-1.30466679482154E-12,1.,0.));
#11681=DIRECTION('ref_axis',(0.,0.,-1.));
#11682=DIRECTION('',(0.5,6.52333397410772E-13,0.866025403784439));
#11683=DIRECTION('center_axis',(0.866025403784439,1.82700839766916E-13,
-0.5));
#11684=DIRECTION('ref_axis',(2.10964758041199E-13,-1.,0.));
#11685=DIRECTION('center_axis',(0.866025403784439,1.82700839766916E-13,
-0.5));
#11686=DIRECTION('ref_axis',(0.5,0.,0.866025403784439));
#11687=DIRECTION('',(-2.10964758041199E-13,1.,0.));
#11688=DIRECTION('center_axis',(0.866025403784439,1.82700839766916E-13,
-0.5));
#11689=DIRECTION('ref_axis',(-0.5,-1.05482379103751E-13,-0.866025403784439));
#11690=DIRECTION('',(-0.5,6.4832235838889E-13,-0.866025403784439));
#11691=DIRECTION('center_axis',(-1.29664471677778E-12,-1.,0.));
#11692=DIRECTION('ref_axis',(-1.,1.29664471677778E-12,0.));
#11693=DIRECTION('center_axis',(-1.29664471677778E-12,-1.,0.));
#11694=DIRECTION('ref_axis',(0.,0.,1.));
#11695=DIRECTION('',(0.,0.,1.));
#11696=DIRECTION('center_axis',(0.,0.,-1.));
#11697=DIRECTION('ref_axis',(0.707106781186895,0.7071067811862,0.));
#11698=DIRECTION('',(0.,0.,1.));
#11699=DIRECTION('center_axis',(-1.35644469630397E-12,-0.866025403784439,
-0.5));
#11700=DIRECTION('ref_axis',(7.8314371117082E-13,0.5,-0.866025403784439));
#11701=DIRECTION('center_axis',(0.,0.,-1.));
#11702=DIRECTION('ref_axis',(0.707106781186895,0.7071067811862,0.));
#11703=DIRECTION('center_axis',(-0.866025403784439,2.42308806056559E-16,
-0.5));
#11704=DIRECTION('ref_axis',(0.5,-1.39897054514259E-16,-0.866025403784439));
#11705=DIRECTION('',(0.,0.,-1.));
#11706=DIRECTION('center_axis',(1.80920256647203E-12,-1.,0.));
#11707=DIRECTION('ref_axis',(-1.,-1.80920256647203E-12,0.));
#11708=DIRECTION('center_axis',(1.80920256647203E-12,-1.,0.));
#11709=DIRECTION('ref_axis',(0.,0.,1.));
#11710=DIRECTION('',(-0.5,-9.04601283236015E-13,0.866025403784439));
#11711=DIRECTION('center_axis',(0.,0.,-1.));
#11712=DIRECTION('ref_axis',(-0.707106781186768,0.707106781186327,0.));
#11713=DIRECTION('center_axis',(0.,0.,-1.));
#11714=DIRECTION('ref_axis',(-0.707106781186768,0.707106781186327,0.));
#11715=DIRECTION('center_axis',(-1.35644469630397E-12,-0.866025403784439,
-0.5));
#11716=DIRECTION('ref_axis',(7.83108736907191E-13,0.5,-0.866025403784439));
#11717=DIRECTION('',(0.,0.,-1.));
#11718=DIRECTION('center_axis',(1.,1.91935343509834E-12,0.));
#11719=DIRECTION('ref_axis',(1.91935343509834E-12,-1.,0.));
#11720=DIRECTION('center_axis',(1.,1.91935343509834E-12,0.));
#11721=DIRECTION('ref_axis',(0.,0.,1.));
#11722=DIRECTION('',(9.59676717549172E-13,-0.5,0.866025403784439));
#11723=DIRECTION('center_axis',(-1.62884833462111E-16,1.,0.));
#11724=DIRECTION('ref_axis',(1.,1.62884833462111E-16,0.));
#11725=DIRECTION('center_axis',(-1.62884833462111E-16,1.,0.));
#11726=DIRECTION('ref_axis',(0.,0.,-1.));
#11727=DIRECTION('',(0.5,8.14424167310554E-17,-0.866025403784439));
#11728=DIRECTION('center_axis',(-0.866025403784439,2.42308806056559E-16,
-0.5));
#11729=DIRECTION('ref_axis',(2.79794108807543E-16,1.,0.));
#11730=DIRECTION('center_axis',(-0.866025403784439,2.42308806056559E-16,
-0.5));
#11731=DIRECTION('ref_axis',(0.5,0.,-0.866025403784439));
#11732=DIRECTION('',(-2.79794108807543E-16,-1.,0.));
#11733=DIRECTION('center_axis',(-0.866025403784439,2.42308806056559E-16,
-0.5));
#11734=DIRECTION('ref_axis',(0.5,0.,-0.866025403784439));
#11735=DIRECTION('center_axis',(-1.,2.79168316070879E-12,0.));
#11736=DIRECTION('ref_axis',(2.79168316070879E-12,1.,0.));
#11737=DIRECTION('center_axis',(-1.,2.79168316070879E-12,0.));
#11738=DIRECTION('ref_axis',(0.,0.,-1.));
#11739=DIRECTION('',(1.3958415803544E-12,0.5,-0.866025403784439));
#11740=DIRECTION('center_axis',(-1.35644469630397E-12,-0.866025403784439,
-0.5));
#11741=DIRECTION('ref_axis',(-1.,1.56628742110387E-12,0.));
#11742=DIRECTION('center_axis',(-1.35644469630397E-12,-0.866025403784439,
-0.5));
#11743=DIRECTION('ref_axis',(0.,-0.5,0.866025403784439));
#11744=DIRECTION('',(1.,-1.56628742110387E-12,0.));
#11745=DIRECTION('center_axis',(0.,0.,-1.));
#11746=DIRECTION('ref_axis',(-1.,0.,0.));
#11747=DIRECTION('center_axis',(0.,0.,-1.));
#11748=DIRECTION('ref_axis',(-1.,0.,0.));
#11749=DIRECTION('center_axis',(0.,0.,-1.));
#11750=DIRECTION('ref_axis',(1.,0.,0.));
#11751=DIRECTION('center_axis',(-1.22464679914735E-16,-1.,0.));
#11752=DIRECTION('ref_axis',(1.,-1.22464679914735E-16,0.));
#11753=DIRECTION('center_axis',(0.,0.,1.));
#11754=DIRECTION('ref_axis',(1.,0.,0.));
#11755=DIRECTION('center_axis',(0.,0.,-1.));
#11756=DIRECTION('ref_axis',(-1.,0.,0.));
#11757=DIRECTION('center_axis',(0.,0.,-1.));
#11758=DIRECTION('ref_axis',(1.,0.,0.));
#11759=DIRECTION('center_axis',(0.,0.,-1.));
#11760=DIRECTION('ref_axis',(-1.,0.,0.));
#11761=DIRECTION('center_axis',(0.,0.,-1.));
#11762=DIRECTION('ref_axis',(1.,0.,0.));
#11763=DIRECTION('',(0.,0.,1.));
#11764=DIRECTION('center_axis',(0.,0.,-1.));
#11765=DIRECTION('ref_axis',(-1.,0.,0.));
#11766=DIRECTION('center_axis',(0.,0.,-1.));
#11767=DIRECTION('ref_axis',(-1.,0.,0.));
#11768=DIRECTION('',(-0.258819045102519,3.16961915143174E-17,0.965925826289069));
#11769=DIRECTION('center_axis',(0.,0.,-1.));
#11770=DIRECTION('ref_axis',(-1.,0.,0.));
#11771=DIRECTION('center_axis',(0.,0.,1.));
#11772=DIRECTION('ref_axis',(-1.,0.,0.));
#11773=DIRECTION('',(0.,0.,1.));
#11774=DIRECTION('center_axis',(0.,0.,-1.));
#11775=DIRECTION('ref_axis',(-1.,0.,0.));
#11776=DIRECTION('center_axis',(6.12323399573676E-17,0.,1.));
#11777=DIRECTION('ref_axis',(1.,0.,0.));
#11778=DIRECTION('center_axis',(1.22464679914735E-16,-1.,0.));
#11779=DIRECTION('ref_axis',(-1.,-1.22464679914735E-16,0.));
#11780=DIRECTION('center_axis',(0.,0.,-1.));
#11781=DIRECTION('ref_axis',(1.,0.,0.));
#11782=DIRECTION('center_axis',(0.,0.,-1.));
#11783=DIRECTION('ref_axis',(1.,0.,0.));
#11784=DIRECTION('center_axis',(0.,0.,-1.));
#11785=DIRECTION('ref_axis',(-1.,0.,0.));
#11786=DIRECTION('',(-0.087155742757872,1.06735001395738E-17,0.996194698090852));
#11787=DIRECTION('',(-2.44029224693388E-18,1.00326855168031E-18,1.));
#11788=DIRECTION('',(1.,6.12380352654702E-33,3.46944695195361E-18));
#11789=DIRECTION('',(-2.44029224693388E-18,1.00326855168031E-18,1.));
#11790=DIRECTION('',(1.,6.12380352654702E-33,3.46944695195361E-18));
#11791=DIRECTION('',(-2.44029224693388E-18,1.00326855168031E-18,1.));
#11792=DIRECTION('',(1.,6.12380352654702E-33,3.46944695195361E-18));
#11793=DIRECTION('',(-2.44029224693388E-18,1.00326855168031E-18,1.));
#11794=DIRECTION('',(1.,6.12380352654702E-33,3.46944695195361E-18));
#11795=DIRECTION('',(-2.44029224693388E-18,1.00326855168031E-18,1.));
#11796=DIRECTION('',(1.,6.12380352654702E-33,3.46944695195361E-18));
#11797=DIRECTION('',(-2.44029224693388E-18,1.00326855168031E-18,1.));
#11798=DIRECTION('',(1.,6.12380352654702E-33,3.46944695195361E-18));
#11799=DIRECTION('',(-2.44029224693388E-18,1.00326855168031E-18,1.));
#11800=DIRECTION('',(1.,6.12380352654702E-33,3.46944695195361E-18));
#11801=DIRECTION('',(-2.44029224693388E-18,1.00326855168031E-18,1.));
#11802=DIRECTION('',(1.,6.12380352654702E-33,3.46944695195361E-18));
#11803=DIRECTION('',(1.,-1.22464679914735E-16,3.46944695195361E-18));
#11804=DIRECTION('',(-2.44029224693388E-18,1.00326855168031E-18,1.));
#11805=DIRECTION('',(1.,-1.22464679914735E-16,3.46944695195361E-18));
#11806=DIRECTION('',(-2.44029224693388E-18,1.00326855168031E-18,1.));
#11807=DIRECTION('',(1.,-1.22464679914735E-16,3.46944695195361E-18));
#11808=DIRECTION('',(-2.44029224693388E-18,1.00326855168031E-18,1.));
#11809=DIRECTION('',(1.,-1.22464679914735E-16,3.46944695195361E-18));
#11810=DIRECTION('',(-2.44029224693388E-18,1.00326855168031E-18,1.));
#11811=CARTESIAN_POINT('',(0.,0.,0.));
#11812=CARTESIAN_POINT('',(0.,0.,0.));
#11813=CARTESIAN_POINT('Origin',(8.5,25.0098518119976,-22.4105093470644));
#11814=CARTESIAN_POINT('',(0.499999999999999,22.2688065021356,-18.8416621089099));
#11815=CARTESIAN_POINT('',(1.74028546827764,22.2688065021356,-18.8416621089099));
#11816=CARTESIAN_POINT('',(8.5,22.2688065021356,-18.8416621089099));
#11817=CARTESIAN_POINT('',(2.74028546827765,21.2688065021356,-19.9095935169016));
#11818=CARTESIAN_POINT('Ctrl Pts',(1.74028546827765,22.2688065021356,-18.8416621089099));
#11819=CARTESIAN_POINT('Ctrl Pts',(1.83421821452936,22.2688065021356,-18.8416621089099));
#11820=CARTESIAN_POINT('Ctrl Pts',(1.93470401993251,22.2546061414744,-18.8524321964904));
#11821=CARTESIAN_POINT('Ctrl Pts',(2.12234108686958,22.1981250134701,-18.8968952198158));
#11822=CARTESIAN_POINT('Ctrl Pts',(2.20951967834708,22.1560062467128,-18.9306784121546));
#11823=CARTESIAN_POINT('Ctrl Pts',(2.38012940236584,22.0462287372975,-19.0232033412094));
#11824=CARTESIAN_POINT('Ctrl Pts',(2.46708450855627,21.9643664133557,-19.0954331993668));
#11825=CARTESIAN_POINT('Ctrl Pts',(2.60062014887845,21.7902127170047,-19.2642996258922));
#11826=CARTESIAN_POINT('Ctrl Pts',(2.64760861619124,21.6983105804248,-19.361014553391));
#11827=CARTESIAN_POINT('Ctrl Pts',(2.72401108672779,21.4919221323301,-19.5980623673013));
#11828=CARTESIAN_POINT('Ctrl Pts',(2.74028546827765,21.3756357329717,-19.7497908605485));
#11829=CARTESIAN_POINT('Ctrl Pts',(2.74028546827765,21.2688065021356,-19.9095935169016));
#11830=CARTESIAN_POINT('',(2.74028546827765,20.5098518119976,-22.4105093470644));
#11831=CARTESIAN_POINT('Origin',(2.74028546827764,25.0098518119976,-22.4105093470644));
#11832=CARTESIAN_POINT('',(6.5,20.5098518119976,-22.4105093470644));
#11833=CARTESIAN_POINT('',(8.5,20.5098518119976,-22.4105093470644));
#11834=CARTESIAN_POINT('',(6.5,25.0098518119976,-17.9105093470644));
#11835=CARTESIAN_POINT('Origin',(6.5,25.0098518119976,-22.4105093470644));
#11836=CARTESIAN_POINT('',(0.499999999999999,25.0098518119976,-17.9105093470644));
#11837=CARTESIAN_POINT('',(8.5,25.0098518119976,-17.9105093470644));
#11838=CARTESIAN_POINT('Origin',(0.499999999999999,25.0098518119976,-22.4105093470644));
#11839=CARTESIAN_POINT('Origin',(8.5,20.5098518119976,-25.0483789742253));
#11840=CARTESIAN_POINT('',(2.74028546827764,20.5098518119976,-23.0483789742253));
#11841=CARTESIAN_POINT('',(2.74028546827765,20.5098518119976,-25.0483789742253));
#11842=CARTESIAN_POINT('',(6.5,20.5098518119976,-23.0483789742253));
#11843=CARTESIAN_POINT('',(1.,20.5098518119976,-23.0483789742253));
#11844=CARTESIAN_POINT('',(6.5,20.5098518119976,-6.56473183187052));
#11845=CARTESIAN_POINT('Origin',(1.74028546827764,22.2688065021356,-25.0483789742253));
#11846=CARTESIAN_POINT('',(-0.5,22.2688065021356,-25.0483789742253));
#11847=CARTESIAN_POINT('',(-0.5,22.2688065021356,-23.0483789742253));
#11848=CARTESIAN_POINT('',(-0.499999999999999,22.2688065021356,-6.56473183187052));
#11849=CARTESIAN_POINT('',(1.74028546827764,22.2688065021356,-25.0483789742253));
#11850=CARTESIAN_POINT('',(-2.37985726586118,22.2688065021356,-25.0483789742253));
#11851=CARTESIAN_POINT('',(1.74028546827764,22.2688065021356,-25.0483789742253));
#11852=CARTESIAN_POINT('',(0.5,22.2688065021356,-23.0483789742253));
#11853=CARTESIAN_POINT('',(0.499999999999999,22.2688065021356,-23.7639115674351));
#11854=CARTESIAN_POINT('',(-2.37985726586118,22.2688065021356,-23.0483789742253));
#11855=CARTESIAN_POINT('Origin',(1.74028546827765,21.2688065021356,-25.0483789742253));
#11856=CARTESIAN_POINT('',(2.74028546827765,21.2688065021356,-25.0483789742253));
#11857=CARTESIAN_POINT('Origin',(1.74028546827765,21.2688065021356,-25.0483789742253));
#11858=CARTESIAN_POINT('',(2.74028546827765,21.2688065021356,-25.0483789742253));
#11859=CARTESIAN_POINT('Origin',(2.74028546827764,17.8031073387245,-25.0483789742253));
#11860=CARTESIAN_POINT('',(2.74028546827764,17.8031073387245,-25.0483789742253));
#11861=CARTESIAN_POINT('',(2.74028546827764,5.68566717807833,-25.0483789742253));
#11862=CARTESIAN_POINT('',(2.74028546827764,17.8031073387245,-23.0483789742253));
#11863=CARTESIAN_POINT('',(2.74028546827764,17.8031073387245,-25.0483789742253));
#11864=CARTESIAN_POINT('',(2.74028546827764,5.68566717807833,-23.0483789742253));
#11865=CARTESIAN_POINT('Origin',(1.74028546827765,17.8031073387245,-25.0483789742253));
#11866=CARTESIAN_POINT('',(1.74028546827765,16.8031073387245,-25.0483789742253));
#11867=CARTESIAN_POINT('Origin',(1.74028546827765,17.8031073387245,-25.0483789742253));
#11868=CARTESIAN_POINT('',(1.74028546827765,16.8031073387245,-23.0483789742253));
#11869=CARTESIAN_POINT('',(1.74028546827765,16.8031073387245,-25.0483789742253));
#11870=CARTESIAN_POINT('Origin',(1.74028546827765,17.8031073387245,-23.0483789742253));
#11871=CARTESIAN_POINT('Origin',(-14.7402854682776,16.8031073387245,-25.0483789742253));
#11872=CARTESIAN_POINT('',(-0.499999999999999,16.8031073387245,-23.0483789742253));
#11873=CARTESIAN_POINT('',(-0.499999999999999,16.8031073387245,-25.0483789742253));
#11874=CARTESIAN_POINT('',(-0.499999999999999,16.8031073387245,-6.56473183187052));
#11875=CARTESIAN_POINT('',(-10.6201427341388,16.8031073387245,-23.0483789742253));
#11876=CARTESIAN_POINT('',(-10.6201427341388,16.8031073387245,-25.0483789742253));
#11877=CARTESIAN_POINT('Origin',(-6.5,-6.43177298256785,-23.0483789742253));
#11878=CARTESIAN_POINT('',(0.499999999999999,23.6522353938789,-23.0483789742253));
#11879=CARTESIAN_POINT('',(0.499999999999999,9.27063275147817,-23.0483789742253));
#11880=CARTESIAN_POINT('',(-0.499999999999999,23.6522353938789,-23.0483789742253));
#11881=CARTESIAN_POINT('',(8.5,23.6522353938789,-23.0483789742253));
#11882=CARTESIAN_POINT('',(-0.499999999999999,1.53522655283679,-23.0483789742253));
#11883=CARTESIAN_POINT('Origin',(-6.5,-6.43177298256785,-23.0483789742253));
#11884=CARTESIAN_POINT('',(-0.499999999999999,-4.64778321739598,-23.0483789742253));
#11885=CARTESIAN_POINT('',(-0.499999999999999,1.53522655283679,-23.0483789742253));
#11886=CARTESIAN_POINT('',(0.499999999999999,-4.64778321739598,-23.0483789742253));
#11887=CARTESIAN_POINT('',(8.5,-4.64778321739598,-23.0483789742253));
#11888=CARTESIAN_POINT('',(0.499999999999998,-1.50539963551477,-23.0483789742253));
#11889=CARTESIAN_POINT('',(0.499999999999999,-6.20017964580458,-23.0483789742253));
#11890=CARTESIAN_POINT('',(6.5,-1.50539963551477,-23.0483789742253));
#11891=CARTESIAN_POINT('',(1.,-1.50539963551477,-23.0483789742253));
#11892=CARTESIAN_POINT('',(6.5,1.53522655283679,-23.0483789742253));
#11893=CARTESIAN_POINT('Origin',(-0.499999999999999,9.50222608824143,11.9189153104842));
#11894=CARTESIAN_POINT('',(-0.499999999999999,-6.43177298256785,-25.0483789742253));
#11895=CARTESIAN_POINT('',(-0.499999999999999,1.53522655283679,-25.0483789742253));
#11896=CARTESIAN_POINT('',(-0.499999999999999,-8.43177298256785,-23.0483789742253));
#11897=CARTESIAN_POINT('Origin',(-0.499999999999999,-6.43177298256785,-23.0483789742253));
#11898=CARTESIAN_POINT('',(-0.499999999999999,-8.43177298256785,46.8862095951938));
#11899=CARTESIAN_POINT('',(-0.499999999999999,-8.43177298256785,30.402562452839));
#11900=CARTESIAN_POINT('',(-0.499999999999999,-6.43177298256785,48.8862095951938));
#11901=CARTESIAN_POINT('Origin',(-0.499999999999999,-6.43177298256785,46.8862095951938));
#11902=CARTESIAN_POINT('',(-0.499999999999999,-5.56822701743215,48.8862095951938));
#11903=CARTESIAN_POINT('',(-0.499999999999999,2.03522655283679,48.8862095951938));
#11904=CARTESIAN_POINT('',(-0.499999999999999,-5.56822701743215,46.8862095951938));
#11905=CARTESIAN_POINT('',(-0.499999999999999,-5.56822701743215,30.402562452839));
#11906=CARTESIAN_POINT('',(-0.499999999999999,-6.43177298256785,46.8862095951938));
#11907=CARTESIAN_POINT('',(-0.499999999999999,15.3987725179725,46.8862095951938));
#11908=CARTESIAN_POINT('',(-0.499999999999999,-6.43177298256785,30.9666314003931));
#11909=CARTESIAN_POINT('',(-0.499999999999999,-6.43177298256785,30.402562452839));
#11910=CARTESIAN_POINT('',(-0.499999999999999,-7.44334688204796,29.5483789742253));
#11911=CARTESIAN_POINT('Origin',(-0.499999999999999,-5.94334688204796,29.5483789742253));
#11912=CARTESIAN_POINT('',(-0.499999999999999,-6.43177298256785,28.1301265480575));
#11913=CARTESIAN_POINT('Origin',(-0.499999999999999,-5.94334688204796,29.5483789742253));
#11914=CARTESIAN_POINT('',(-0.499999999999999,-6.43177298256785,-20.9723835636495));
#11915=CARTESIAN_POINT('',(-0.499999999999999,-6.43177298256785,30.402562452839));
#11916=CARTESIAN_POINT('',(-0.499999999999999,-7.50539963551477,-22.4105093470644));
#11917=CARTESIAN_POINT('Origin',(-0.499999999999999,-6.00539963551477,-22.4105093470644));
#11918=CARTESIAN_POINT('Origin',(-0.499999999999999,-6.00539963551477,-22.4105093470644));
#11919=CARTESIAN_POINT('Origin',(1.,-7.43177298256785,-18.9105093470644));
#11920=CARTESIAN_POINT('',(7.5,-7.43177298256785,-19.9105093470644));
#11921=CARTESIAN_POINT('',(7.5,-8.43177298256785,-18.9105093470644));
#11922=CARTESIAN_POINT('Origin',(7.5,-7.43177298256785,-18.9105093470644));
#11923=CARTESIAN_POINT('',(2.5,-8.43177298256785,-18.9105093470644));
#11924=CARTESIAN_POINT('',(1.,-8.43177298256785,-18.9105093470644));
#11925=CARTESIAN_POINT('',(2.5,-7.43177298256785,-19.9105093470644));
#11926=CARTESIAN_POINT('Origin',(2.5,-7.43177298256785,-18.9105093470644));
#11927=CARTESIAN_POINT('',(1.,-7.43177298256785,-19.9105093470644));
#11928=CARTESIAN_POINT('Origin',(7.5,21.5098518119976,-6.56473183187052));
#11929=CARTESIAN_POINT('',(7.5,22.5098518119976,-25.0483789742253));
#11930=CARTESIAN_POINT('',(7.5,22.5098518119976,-22.4105093470644));
#11931=CARTESIAN_POINT('',(7.5,22.5098518119976,-6.56473183187052));
#11932=CARTESIAN_POINT('',(8.5,21.5098518119976,-22.4105093470644));
#11933=CARTESIAN_POINT('Origin',(7.5,21.5098518119976,-22.4105093470644));
#11934=CARTESIAN_POINT('',(8.5,21.5098518119976,-24.0483789742253));
#11935=CARTESIAN_POINT('',(8.5,21.5098518119976,-6.56473183187052));
#11936=CARTESIAN_POINT('Origin',(7.5,21.5098518119976,-24.0483789742253));
#11937=CARTESIAN_POINT('Origin',(7.5,1.53522655283679,-24.0483789742253));
#11938=CARTESIAN_POINT('',(8.5,-2.50539963551477,-24.0483789742253));
#11939=CARTESIAN_POINT('',(8.5,1.53522655283679,-24.0483789742253));
#11940=CARTESIAN_POINT('',(7.5,-3.50539963551477,-25.0483789742253));
#11941=CARTESIAN_POINT('Origin',(7.5,-2.50539963551477,-24.0483789742253));
#11942=CARTESIAN_POINT('',(7.5,1.53522655283679,-25.0483789742253));
#11943=CARTESIAN_POINT('Origin',(7.5,0.535226552836792,-18.9105093470644));
#11944=CARTESIAN_POINT('',(8.5,-7.43177298256785,-18.9105093470644));
#11945=CARTESIAN_POINT('Origin',(7.5,-7.43177298256785,-18.9105093470644));
#11946=CARTESIAN_POINT('',(7.5,-6.00539963551477,-19.9105093470644));
#11947=CARTESIAN_POINT('',(7.5,0.535226552836792,-19.9105093470644));
#11948=CARTESIAN_POINT('',(8.5,-6.00539963551477,-18.9105093470644));
#11949=CARTESIAN_POINT('Origin',(7.5,-6.00539963551477,-18.9105093470644));
#11950=CARTESIAN_POINT('',(8.5,0.535226552836792,-18.9105093470644));
#11951=CARTESIAN_POINT('Origin',(7.5,-6.00539963551477,-22.4105093470644));
#11952=CARTESIAN_POINT('',(7.5,-3.50539963551477,-22.4105093470644));
#11953=CARTESIAN_POINT('',(8.5,-2.50539963551477,-22.4105093470644));
#11954=CARTESIAN_POINT('Origin',(7.5,-2.50539963551477,-22.4105093470644));
#11955=CARTESIAN_POINT('Origin',(8.5,-6.00539963551477,-22.4105093470644));
#11956=CARTESIAN_POINT('Origin',(7.5,-6.00539963551477,-22.4105093470644));
#11957=CARTESIAN_POINT('Origin',(7.5,-2.50539963551477,-5.2457970182901));
#11958=CARTESIAN_POINT('',(8.5,-2.50539963551477,-5.2457970182901));
#11959=CARTESIAN_POINT('',(7.5,-3.50539963551477,-5.2457970182901));
#11960=CARTESIAN_POINT('Origin',(7.5,25.0098518119976,-22.4105093470644));
#11961=CARTESIAN_POINT('',(7.5,25.0098518119976,-19.9105093470644));
#11962=CARTESIAN_POINT('',(8.5,25.0098518119976,-18.9105093470644));
#11963=CARTESIAN_POINT('Origin',(7.5,25.0098518119976,-18.9105093470644));
#11964=CARTESIAN_POINT('Origin',(8.5,25.0098518119976,-22.4105093470644));
#11965=CARTESIAN_POINT('Origin',(7.5,25.0098518119976,-22.4105093470644));
#11966=CARTESIAN_POINT('Origin',(7.5,17.2560389501195,-18.9105093470644));
#11967=CARTESIAN_POINT('',(7.5,26.4362251590507,-19.9105093470644));
#11968=CARTESIAN_POINT('',(8.5,26.4362251590507,-18.9105093470644));
#11969=CARTESIAN_POINT('Origin',(7.5,26.4362251590507,-18.9105093470644));
#11970=CARTESIAN_POINT('',(8.5,17.2560389501195,-18.9105093470644));
#11971=CARTESIAN_POINT('',(7.5,17.2560389501195,-19.9105093470644));
#11972=CARTESIAN_POINT('Origin',(7.5,-7.43177298256785,-18.9105093470644));
#11973=CARTESIAN_POINT('Origin',(7.5,-7.43177298256785,-18.9105093470644));
#11974=CARTESIAN_POINT('Origin',(1.,26.4362251590507,-18.9105093470644));
#11975=CARTESIAN_POINT('',(7.5,27.4362251590507,-18.9105093470644));
#11976=CARTESIAN_POINT('Origin',(7.5,26.4362251590507,-18.9105093470644));
#11977=CARTESIAN_POINT('',(2.5,26.4362251590507,-19.9105093470644));
#11978=CARTESIAN_POINT('',(1.,26.4362251590507,-19.9105093470644));
#11979=CARTESIAN_POINT('',(2.5,27.4362251590507,-18.9105093470644));
#11980=CARTESIAN_POINT('Origin',(2.5,26.4362251590507,-18.9105093470644));
#11981=CARTESIAN_POINT('',(1.,27.4362251590507,-18.9105093470644));
#11982=CARTESIAN_POINT('Origin',(7.5,26.4362251590507,-18.9105093470644));
#11983=CARTESIAN_POINT('Origin',(7.5,26.4362251590507,-18.9105093470644));
#11984=CARTESIAN_POINT('Origin',(-6.5,-8.43177298256785,48.8862095951938));
#11985=CARTESIAN_POINT('',(2.5,-8.43177298256785,-23.0483789742253));
#11986=CARTESIAN_POINT('',(2.5,-8.43177298256785,13.2033827172745));
#11987=CARTESIAN_POINT('',(7.5,-8.43177298256785,26.0483789742253));
#11988=CARTESIAN_POINT('',(7.5,-8.43177298256785,30.402562452839));
#11989=CARTESIAN_POINT('',(2.5,-8.43177298256785,26.0483789742253));
#11990=CARTESIAN_POINT('',(1.,-8.43177298256785,26.0483789742253));
#11991=CARTESIAN_POINT('',(2.5,-8.43177298256785,33.0483789742253));
#11992=CARTESIAN_POINT('',(2.5,-8.43177298256785,39.2172942847095));
#11993=CARTESIAN_POINT('',(7.5,-8.43177298256785,33.0483789742253));
#11994=CARTESIAN_POINT('',(1.,-8.43177298256785,33.0483789742253));
#11995=CARTESIAN_POINT('',(7.5,-8.43177298256785,46.8862095951938));
#11996=CARTESIAN_POINT('',(7.5,-8.43177298256785,30.402562452839));
#11997=CARTESIAN_POINT('',(-6.5,-8.43177298256785,46.8862095951938));
#11998=CARTESIAN_POINT('',(-6.5,-8.43177298256785,-23.0483789742253));
#11999=CARTESIAN_POINT('Origin',(7.5,-7.43177298256785,30.402562452839));
#12000=CARTESIAN_POINT('',(8.5,-7.43177298256785,26.0483789742253));
#12001=CARTESIAN_POINT('',(8.5,-7.43177298256785,30.402562452839));
#12002=CARTESIAN_POINT('Origin',(7.5,-7.43177298256785,26.0483789742253));
#12003=CARTESIAN_POINT('Origin',(8.5,9.50222608824143,11.9189153104842));
#12004=CARTESIAN_POINT('',(8.5,26.4362251590507,26.0483789742253));
#12005=CARTESIAN_POINT('',(8.5,26.4362251590507,-5.56473183187052));
#12006=CARTESIAN_POINT('',(8.5,24.9477990585308,26.0483789742253));
#12007=CARTESIAN_POINT('',(8.5,18.4692256236461,26.0483789742253));
#12008=CARTESIAN_POINT('',(8.5,21.7971476937744,31.0726479720595));
#12009=CARTESIAN_POINT('Origin',(8.5,24.9477990585308,29.5483789742253));
#12010=CARTESIAN_POINT('',(8.5,20.2953189477035,33.0096109045284));
#12011=CARTESIAN_POINT('Origin',(8.5,22.2953189477035,33.0096109045284));
#12012=CARTESIAN_POINT('',(8.5,20.2953189477035,46.8862095951938));
#12013=CARTESIAN_POINT('',(8.5,20.2953189477035,22.4642631075063));
#12014=CARTESIAN_POINT('',(8.5,19.2953189477036,47.8862095951938));
#12015=CARTESIAN_POINT('Origin',(8.5,19.2953189477036,46.8862095951938));
#12016=CARTESIAN_POINT('',(8.5,-6.43177298256785,47.8862095951938));
#12017=CARTESIAN_POINT('',(8.5,15.3987725179725,47.8862095951938));
#12018=CARTESIAN_POINT('',(8.5,-7.43177298256785,46.8862095951938));
#12019=CARTESIAN_POINT('Origin',(8.5,-6.43177298256785,46.8862095951938));
#12020=CARTESIAN_POINT('',(8.5,-7.43177298256785,33.0483789742253));
#12021=CARTESIAN_POINT('',(8.5,-7.43177298256785,30.402562452839));
#12022=CARTESIAN_POINT('',(8.5,-5.94334688204796,33.0483789742253));
#12023=CARTESIAN_POINT('',(8.5,0.535226552836791,33.0483789742253));
#12024=CARTESIAN_POINT('',(8.5,-5.94334688204796,26.0483789742253));
#12025=CARTESIAN_POINT('Origin',(8.5,-5.94334688204796,29.5483789742253));
#12026=CARTESIAN_POINT('',(8.5,1.77943960309674,26.0483789742253));
#12027=CARTESIAN_POINT('Origin',(7.5,26.4362251590507,-5.56473183187052));
#12028=CARTESIAN_POINT('',(7.5,27.4362251590507,26.0483789742253));
#12029=CARTESIAN_POINT('',(7.5,27.4362251590507,-5.56473183187052));
#12030=CARTESIAN_POINT('Origin',(7.5,26.4362251590507,26.0483789742253));
#12031=CARTESIAN_POINT('Origin',(-6.5,27.4362251590507,-23.0483789742253));
#12032=CARTESIAN_POINT('',(2.5,27.4362251590507,-23.0483789742253));
#12033=CARTESIAN_POINT('',(2.5,27.4362251590507,-22.7639115674351));
#12034=CARTESIAN_POINT('',(-0.499999999999999,27.4362251590507,-23.0483789742253));
#12035=CARTESIAN_POINT('',(-6.5,27.4362251590507,-23.0483789742253));
#12036=CARTESIAN_POINT('',(-0.499999999999999,27.4362251590507,30.0096109045284));
#12037=CARTESIAN_POINT('',(-0.499999999999999,27.4362251590507,-5.56473183187052));
#12038=CARTESIAN_POINT('',(2.5,27.4362251590507,30.0096109045284));
#12039=CARTESIAN_POINT('',(-6.5,27.4362251590507,30.0096109045284));
#12040=CARTESIAN_POINT('',(2.5,27.4362251590507,26.0483789742253));
#12041=CARTESIAN_POINT('',(2.5,27.4362251590507,3.24030798257579));
#12042=CARTESIAN_POINT('',(1.,27.4362251590507,26.0483789742253));
#12043=CARTESIAN_POINT('Origin',(-16.5,18.4317729825679,48.8862095951938));
#12044=CARTESIAN_POINT('',(3.5,18.4317729825679,46.8862095951938));
#12045=CARTESIAN_POINT('',(-0.499999999999999,18.4317729825679,46.8862095951938));
#12046=CARTESIAN_POINT('',(-11.5,18.4317729825679,46.8862095951938));
#12047=CARTESIAN_POINT('',(3.5,18.4317729825679,48.8862095951938));
#12048=CARTESIAN_POINT('',(3.5,18.4317729825679,48.8862095951938));
#12049=CARTESIAN_POINT('',(-0.499999999999999,18.4317729825679,48.8862095951938));
#12050=CARTESIAN_POINT('',(-11.5,18.4317729825679,48.8862095951938));
#12051=CARTESIAN_POINT('',(-0.499999999999999,18.4317729825679,30.402562452839));
#12052=CARTESIAN_POINT('Origin',(5.5,16.4317729825678,48.8862095951938));
#12053=CARTESIAN_POINT('',(5.5,-3.56822701743215,46.8862095951938));
#12054=CARTESIAN_POINT('',(5.5,16.4317729825678,46.8862095951938));
#12055=CARTESIAN_POINT('',(5.5,18.8635459651357,46.8862095951938));
#12056=CARTESIAN_POINT('',(5.5,-3.56822701743215,48.8862095951938));
#12057=CARTESIAN_POINT('',(5.5,-3.56822701743215,48.8862095951938));
#12058=CARTESIAN_POINT('',(5.5,16.4317729825678,48.8862095951938));
#12059=CARTESIAN_POINT('',(5.5,18.8635459651357,48.8862095951938));
#12060=CARTESIAN_POINT('',(5.5,16.4317729825678,48.8862095951938));
#12061=CARTESIAN_POINT('Origin',(3.5,16.4317729825679,48.8862095951938));
#12062=CARTESIAN_POINT('Origin',(3.5,16.4317729825679,46.8862095951938));
#12063=CARTESIAN_POINT('Origin',(3.5,16.4317729825679,48.8862095951938));
#12064=CARTESIAN_POINT('Origin',(3.5,-5.56822701743215,48.8862095951938));
#12065=CARTESIAN_POINT('',(3.5,-5.56822701743215,46.8862095951938));
#12066=CARTESIAN_POINT('',(-1.5,-5.56822701743215,46.8862095951938));
#12067=CARTESIAN_POINT('',(3.5,-5.56822701743215,48.8862095951938));
#12068=CARTESIAN_POINT('',(-1.5,-5.56822701743215,48.8862095951938));
#12069=CARTESIAN_POINT('',(3.5,-5.56822701743215,48.8862095951938));
#12070=CARTESIAN_POINT('Origin',(3.5,-3.56822701743215,48.8862095951938));
#12071=CARTESIAN_POINT('Origin',(3.5,-3.56822701743215,46.8862095951938));
#12072=CARTESIAN_POINT('Origin',(3.5,-3.56822701743215,48.8862095951938));
#12073=CARTESIAN_POINT('Origin',(-6.5,21.2953189477036,48.8862095951938));
#12074=CARTESIAN_POINT('',(7.5,-6.43177298256785,48.8862095951938));
#12075=CARTESIAN_POINT('',(-6.5,-6.43177298256785,48.8862095951938));
#12076=CARTESIAN_POINT('',(7.5,19.2953189477036,48.8862095951938));
#12077=CARTESIAN_POINT('',(7.5,15.3987725179725,48.8862095951938));
#12078=CARTESIAN_POINT('',(-0.499999999999999,19.2953189477036,48.8862095951938));
#12079=CARTESIAN_POINT('',(-6.5,19.2953189477036,48.8862095951938));
#12080=CARTESIAN_POINT('',(-0.499999999999999,2.03522655283679,48.8862095951938));
#12081=CARTESIAN_POINT('Origin',(-0.499999999999999,9.50222608824143,11.9189153104842));
#12082=CARTESIAN_POINT('',(-0.499999999999999,25.4362251590507,-20.9723835636495));
#12083=CARTESIAN_POINT('Origin',(-0.499999999999999,25.0098518119976,-22.4105093470644));
#12084=CARTESIAN_POINT('',(-0.499999999999999,25.4362251590507,28.1301265480575));
#12085=CARTESIAN_POINT('',(-0.499999999999999,25.4362251590507,-5.56473183187052));
#12086=CARTESIAN_POINT('',(-0.499999999999999,23.5204710981556,30.0096109045284));
#12087=CARTESIAN_POINT('Origin',(-0.499999999999999,24.9477990585308,29.5483789742253));
#12088=CARTESIAN_POINT('',(-0.499999999999999,22.2953189477036,30.0096109045284));
#12089=CARTESIAN_POINT('',(-0.499999999999999,17.4692256236461,30.0096109045284));
#12090=CARTESIAN_POINT('',(-0.499999999999999,19.2953189477036,33.0096109045284));
#12091=CARTESIAN_POINT('Origin',(-0.499999999999999,22.2953189477035,33.0096109045284));
#12092=CARTESIAN_POINT('',(-0.499999999999999,19.2953189477036,46.8862095951938));
#12093=CARTESIAN_POINT('',(-0.499999999999999,19.2953189477035,22.4642631075063));
#12094=CARTESIAN_POINT('',(-0.499999999999999,15.3987725179725,46.8862095951938));
#12095=CARTESIAN_POINT('',(-0.499999999999999,21.2953189477036,46.8862095951938));
#12096=CARTESIAN_POINT('Origin',(-0.499999999999999,19.2953189477036,46.8862095951938));
#12097=CARTESIAN_POINT('',(-0.499999999999999,21.2953189477036,33.0096109045284));
#12098=CARTESIAN_POINT('',(-0.499999999999999,21.2953189477035,22.4642631075063));
#12099=CARTESIAN_POINT('',(-0.499999999999999,22.2953189477036,32.0096109045284));
#12100=CARTESIAN_POINT('Origin',(-0.499999999999999,22.2953189477035,33.0096109045284));
#12101=CARTESIAN_POINT('',(-0.499999999999999,25.4362251590507,32.0096109045284));
#12102=CARTESIAN_POINT('',(-0.499999999999999,17.4692256236461,32.0096109045284));
#12103=CARTESIAN_POINT('Origin',(-0.499999999999999,25.4362251590507,30.0096109045284));
#12104=CARTESIAN_POINT('',(-0.499999999999999,25.4362251590507,-25.0483789742253));
#12105=CARTESIAN_POINT('Origin',(-0.499999999999999,25.4362251590507,-23.0483789742253));
#12106=CARTESIAN_POINT('',(-0.499999999999999,1.53522655283679,-25.0483789742253));
#12107=CARTESIAN_POINT('Origin',(8.5,24.9477990585308,29.5483789742253));
#12108=CARTESIAN_POINT('',(2.5,23.4477990585308,29.5483789742253));
#12109=CARTESIAN_POINT('Origin',(2.5,24.9477990585308,29.5483789742253));
#12110=CARTESIAN_POINT('',(0.499999999999999,23.4477990585308,29.5483789742253));
#12111=CARTESIAN_POINT('',(8.5,23.4477990585308,29.5483789742253));
#12112=CARTESIAN_POINT('',(0.499999999999999,23.5204710981556,30.0096109045284));
#12113=CARTESIAN_POINT('Origin',(0.499999999999999,24.9477990585308,29.5483789742253));
#12114=CARTESIAN_POINT('',(8.5,23.5204710981556,30.0096109045284));
#12115=CARTESIAN_POINT('',(0.499999999999999,25.4362251590507,28.1301265480575));
#12116=CARTESIAN_POINT('',(8.5,25.4362251590507,28.1301265480575));
#12117=CARTESIAN_POINT('Origin',(0.499999999999999,24.9477990585308,29.5483789742253));
#12118=CARTESIAN_POINT('Origin',(8.5,25.0098518119976,-22.4105093470644));
#12119=CARTESIAN_POINT('',(2.5,23.5098518119976,-22.4105093470644));
#12120=CARTESIAN_POINT('Origin',(2.5,25.0098518119976,-22.4105093470644));
#12121=CARTESIAN_POINT('',(0.499999999999999,23.5098518119976,-22.4105093470644));
#12122=CARTESIAN_POINT('',(8.5,23.5098518119976,-22.4105093470644));
#12123=CARTESIAN_POINT('',(0.499999999999999,25.4362251590507,-20.9723835636495));
#12124=CARTESIAN_POINT('Origin',(0.499999999999999,25.0098518119976,-22.4105093470644));
#12125=CARTESIAN_POINT('',(8.5,25.4362251590507,-20.9723835636495));
#12126=CARTESIAN_POINT('Origin',(0.499999999999999,25.0098518119976,-22.4105093470644));
#12127=CARTESIAN_POINT('Origin',(8.5,-5.94334688204796,29.5483789742253));
#12128=CARTESIAN_POINT('',(2.5,-7.44334688204796,29.5483789742253));
#12129=CARTESIAN_POINT('Origin',(2.5,-5.94334688204796,29.5483789742253));
#12130=CARTESIAN_POINT('',(8.5,-7.44334688204796,29.5483789742253));
#12131=CARTESIAN_POINT('',(0.499999999999999,-6.43177298256785,30.9666314003931));
#12132=CARTESIAN_POINT('',(8.5,-6.43177298256785,30.9666314003931));
#12133=CARTESIAN_POINT('',(0.499999999999999,-6.43177298256785,28.1301265480575));
#12134=CARTESIAN_POINT('Origin',(0.499999999999999,-5.94334688204796,29.5483789742253));
#12135=CARTESIAN_POINT('',(8.5,-6.43177298256785,28.1301265480575));
#12136=CARTESIAN_POINT('Origin',(8.5,-6.00539963551477,-22.4105093470644));
#12137=CARTESIAN_POINT('',(2.5,-7.50539963551477,-22.4105093470644));
#12138=CARTESIAN_POINT('Origin',(2.5,-6.00539963551477,-22.4105093470644));
#12139=CARTESIAN_POINT('',(8.5,-7.50539963551477,-22.4105093470644));
#12140=CARTESIAN_POINT('',(0.499999999999999,-6.43177298256785,-20.9723835636495));
#12141=CARTESIAN_POINT('',(8.5,-6.43177298256785,-20.9723835636495));
#12142=CARTESIAN_POINT('Origin',(0.499999999999999,-6.00539963551477,-22.4105093470644));
#12143=CARTESIAN_POINT('Origin',(-6.5,25.4362251590507,30.0096109045284));
#12144=CARTESIAN_POINT('',(0.499999999999999,22.2953189477036,30.0096109045284));
#12145=CARTESIAN_POINT('',(0.499999999999999,25.1891186339208,30.0096109045284));
#12146=CARTESIAN_POINT('',(-6.5,22.2953189477036,30.0096109045284));
#12147=CARTESIAN_POINT('Origin',(0.499999999999999,24.9730384855242,-22.4794441606449));
#12148=CARTESIAN_POINT('',(0.499999999999998,25.4362251590507,-17.9105093470644));
#12149=CARTESIAN_POINT('',(0.499999999999999,24.9914451487609,-17.9105093470644));
#12150=CARTESIAN_POINT('',(0.499999999999999,25.4362251590507,3.24030798257579));
#12151=CARTESIAN_POINT('Origin',(0.499999999999999,24.9420121087908,29.5289949393769));
#12152=CARTESIAN_POINT('',(0.499999999999999,-6.43177298256785,34.0483789742253));
#12153=CARTESIAN_POINT('',(0.499999999999999,-6.43177298256785,39.2172942847095));
#12154=CARTESIAN_POINT('',(0.499999999999999,-5.94334688204796,34.0483789742253));
#12155=CARTESIAN_POINT('',(0.499999999999999,-7.18466645743788,34.0483789742253));
#12156=CARTESIAN_POINT('',(0.499999999999999,-5.94334688204796,25.0483789742253));
#12157=CARTESIAN_POINT('Origin',(0.499999999999999,-5.94334688204796,29.5483789742253));
#12158=CARTESIAN_POINT('',(0.499999999999999,-6.43177298256785,25.0483789742253));
#12159=CARTESIAN_POINT('',(0.499999999999999,-5.94045340717793,25.0483789742253));
#12160=CARTESIAN_POINT('',(0.499999999999999,-6.43177298256785,39.2172942847095));
#12161=CARTESIAN_POINT('Origin',(-6.5,-6.43177298256785,48.8862095951938));
#12162=CARTESIAN_POINT('',(6.5,-6.43177298256785,46.8862095951938));
#12163=CARTESIAN_POINT('',(-6.5,-6.43177298256785,46.8862095951938));
#12164=CARTESIAN_POINT('',(6.5,-6.43177298256785,34.0483789742253));
#12165=CARTESIAN_POINT('',(6.5,-6.43177298256785,30.402562452839));
#12166=CARTESIAN_POINT('',(1.,-6.43177298256785,34.0483789742253));
#12167=CARTESIAN_POINT('Origin',(-6.5,-6.43177298256785,48.8862095951938));
#12168=CARTESIAN_POINT('',(6.5,-6.43177298256785,25.0483789742253));
#12169=CARTESIAN_POINT('',(1.,-6.43177298256785,25.0483789742253));
#12170=CARTESIAN_POINT('',(6.5,-6.43177298256785,-17.9105093470644));
#12171=CARTESIAN_POINT('',(6.5,-6.43177298256785,30.402562452839));
#12172=CARTESIAN_POINT('',(0.499999999999998,-6.43177298256785,-17.9105093470644));
#12173=CARTESIAN_POINT('',(1.,-6.43177298256785,-17.9105093470644));
#12174=CARTESIAN_POINT('',(0.499999999999999,-6.43177298256785,13.2033827172745));
#12175=CARTESIAN_POINT('Origin',(8.5,-8.43177298256785,34.0483789742253));
#12176=CARTESIAN_POINT('',(6.5,-5.94334688204796,34.0483789742253));
#12177=CARTESIAN_POINT('',(6.5,0.535226552836791,34.0483789742253));
#12178=CARTESIAN_POINT('',(8.5,-5.94334688204796,34.0483789742253));
#12179=CARTESIAN_POINT('Origin',(-6.5,21.2953189477036,46.8862095951938));
#12180=CARTESIAN_POINT('',(6.5,19.2953189477036,46.8862095951938));
#12181=CARTESIAN_POINT('',(-6.5,19.2953189477036,46.8862095951938));
#12182=CARTESIAN_POINT('',(6.5,15.3987725179725,46.8862095951938));
#12183=CARTESIAN_POINT('Origin',(6.5,9.50222608824143,11.9189153104842));
#12184=CARTESIAN_POINT('',(6.5,20.5630459545133,30.5602782858212));
#12185=CARTESIAN_POINT('',(6.5,24.9477990585308,25.0483789742253));
#12186=CARTESIAN_POINT('Origin',(6.5,24.9477990585308,29.5483789742253));
#12187=CARTESIAN_POINT('',(6.5,25.4362251590507,25.0483789742253));
#12188=CARTESIAN_POINT('',(6.5,18.4692256236461,25.0483789742253));
#12189=CARTESIAN_POINT('',(6.5,25.4362251590507,-17.9105093470644));
#12190=CARTESIAN_POINT('',(6.5,25.4362251590507,-5.56473183187052));
#12191=CARTESIAN_POINT('',(6.5,17.2560389501195,-17.9105093470644));
#12192=CARTESIAN_POINT('',(6.5,-1.50539963551477,-22.4105093470644));
#12193=CARTESIAN_POINT('',(6.5,-1.50539963551477,-5.2457970182901));
#12194=CARTESIAN_POINT('',(6.5,-6.00539963551477,-17.9105093470644));
#12195=CARTESIAN_POINT('Origin',(6.5,-6.00539963551477,-22.4105093470644));
#12196=CARTESIAN_POINT('',(6.5,0.535226552836792,-17.9105093470644));
#12197=CARTESIAN_POINT('',(6.5,-5.94334688204796,25.0483789742253));
#12198=CARTESIAN_POINT('',(6.5,18.4692256236461,25.0483789742253));
#12199=CARTESIAN_POINT('Origin',(6.5,-5.94334688204796,29.5483789742253));
#12200=CARTESIAN_POINT('',(6.5,19.2953189477036,33.0096109045284));
#12201=CARTESIAN_POINT('',(6.5,19.2953189477035,22.4642631075063));
#12202=CARTESIAN_POINT('Origin',(6.5,22.2953189477035,33.0096109045284));
#12203=CARTESIAN_POINT('Origin',(-6.5,19.2953189477036,33.0096109045284));
#12204=CARTESIAN_POINT('',(-6.5,19.2953189477036,33.0096109045284));
#12205=CARTESIAN_POINT('Origin',(-6.5,22.2953189477035,33.0096109045284));
#12206=CARTESIAN_POINT('',(0.499999999999999,20.5630459545133,30.5602782858212));
#12207=CARTESIAN_POINT('Origin',(0.499999999999999,22.2953189477035,33.0096109045284));
#12208=CARTESIAN_POINT('',(8.5,20.5630459545133,30.5602782858212));
#12209=CARTESIAN_POINT('Origin',(8.5,24.9477990585308,29.5483789742253));
#12210=CARTESIAN_POINT('',(0.499999999999999,24.9477990585308,25.0483789742253));
#12211=CARTESIAN_POINT('Origin',(0.499999999999999,24.9477990585308,29.5483789742253));
#12212=CARTESIAN_POINT('',(8.5,24.9477990585308,25.0483789742253));
#12213=CARTESIAN_POINT('Origin',(8.5,27.4362251590507,25.0483789742253));
#12214=CARTESIAN_POINT('',(8.5,-5.94334688204796,25.0483789742253));
#12215=CARTESIAN_POINT('Origin',(8.5,27.4362251590507,25.0483789742253));
#12216=CARTESIAN_POINT('',(0.499999999999999,25.4362251590507,25.0483789742253));
#12217=CARTESIAN_POINT('',(0.499999999999999,26.1891186339208,25.0483789742253));
#12218=CARTESIAN_POINT('',(1.,25.4362251590507,25.0483789742253));
#12219=CARTESIAN_POINT('Origin',(0.499999999999999,24.9420121087908,29.5289949393769));
#12220=CARTESIAN_POINT('',(0.499999999999999,25.4362251590507,3.24030798257579));
#12221=CARTESIAN_POINT('Origin',(-6.5,25.4362251590507,-23.0483789742253));
#12222=CARTESIAN_POINT('',(1.,25.4362251590507,-17.9105093470644));
#12223=CARTESIAN_POINT('Origin',(8.5,-5.94334688204796,29.5483789742253));
#12224=CARTESIAN_POINT('Origin',(8.5,25.0098518119976,-17.9105093470644));
#12225=CARTESIAN_POINT('',(0.499999999999999,-6.00539963551477,-17.9105093470644));
#12226=CARTESIAN_POINT('',(8.5,-6.00539963551477,-17.9105093470644));
#12227=CARTESIAN_POINT('',(0.499999999999999,-7.20017964580458,-17.9105093470644));
#12228=CARTESIAN_POINT('Origin',(8.5,-1.50539963551477,-22.4105093470644));
#12229=CARTESIAN_POINT('',(0.499999999999999,-1.50539963551477,-22.4105093470644));
#12230=CARTESIAN_POINT('',(0.499999999999999,-1.50539963551477,-22.4449767538547));
#12231=CARTESIAN_POINT('',(8.5,-1.50539963551477,-22.4105093470644));
#12232=CARTESIAN_POINT('Origin',(8.5,-6.00539963551477,-22.4105093470644));
#12233=CARTESIAN_POINT('Origin',(0.499999999999999,-6.00539963551477,-22.4105093470644));
#12234=CARTESIAN_POINT('Origin',(0.499999999999999,-5.96858630904131,-22.4794441606449));
#12235=CARTESIAN_POINT('Origin',(8.5,25.0098518119976,-17.9105093470644));
#12236=CARTESIAN_POINT('Origin',(7.5,0.535226552836791,33.0483789742253));
#12237=CARTESIAN_POINT('',(7.5,-7.43177298256785,32.0483789742253));
#12238=CARTESIAN_POINT('Origin',(7.5,-7.43177298256785,33.0483789742253));
#12239=CARTESIAN_POINT('',(7.5,-5.94334688204796,32.0483789742253));
#12240=CARTESIAN_POINT('',(7.5,0.535226552836791,32.0483789742253));
#12241=CARTESIAN_POINT('Origin',(7.5,-5.94334688204796,33.0483789742253));
#12242=CARTESIAN_POINT('Origin',(7.5,-5.94334688204796,29.5483789742253));
#12243=CARTESIAN_POINT('',(7.5,-5.94334688204796,27.0483789742253));
#12244=CARTESIAN_POINT('Origin',(7.5,-5.94334688204796,26.0483789742253));
#12245=CARTESIAN_POINT('Origin',(7.5,-5.94334688204796,29.5483789742253));
#12246=CARTESIAN_POINT('Origin',(7.5,1.77943960309674,26.0483789742253));
#12247=CARTESIAN_POINT('',(7.5,-7.43177298256785,27.0483789742253));
#12248=CARTESIAN_POINT('Origin',(7.5,-7.43177298256785,26.0483789742253));
#12249=CARTESIAN_POINT('',(7.5,1.77943960309674,27.0483789742253));
#12250=CARTESIAN_POINT('Origin',(7.5,22.2953189477035,33.0096109045284));
#12251=CARTESIAN_POINT('',(7.5,22.046233320739,32.041129438294));
#12252=CARTESIAN_POINT('Origin',(7.5,21.7971476937744,31.0726479720595));
#12253=CARTESIAN_POINT('',(7.5,21.2953189477036,33.0096109045284));
#12254=CARTESIAN_POINT('Origin',(7.5,22.2953189477035,33.0096109045284));
#12255=CARTESIAN_POINT('Origin',(7.5,20.2953189477035,33.0096109045284));
#12256=CARTESIAN_POINT('Origin',(7.5,20.2953189477035,22.4642631075063));
#12257=CARTESIAN_POINT('',(7.5,21.2953189477036,46.8862095951938));
#12258=CARTESIAN_POINT('Origin',(7.5,20.2953189477035,46.8862095951938));
#12259=CARTESIAN_POINT('',(7.5,21.2953189477035,22.4642631075063));
#12260=CARTESIAN_POINT('Ctrl Pts',(8.5,19.2953189477036,47.8862095951938));
#12261=CARTESIAN_POINT('Ctrl Pts',(8.5,20.2953189477035,47.8862095951938));
#12262=CARTESIAN_POINT('Ctrl Pts',(8.5,20.2953189477035,46.8862095951938));
#12263=CARTESIAN_POINT('Ctrl Pts',(8.5,19.2953189477036,48.8862095951938));
#12264=CARTESIAN_POINT('Ctrl Pts',(8.5,21.2953189477035,48.8862095951938));
#12265=CARTESIAN_POINT('Ctrl Pts',(8.5,21.2953189477035,46.8862095951938));
#12266=CARTESIAN_POINT('Ctrl Pts',(7.5,19.2953189477036,48.8862095951938));
#12267=CARTESIAN_POINT('Ctrl Pts',(7.5,21.2953189477035,48.8862095951938));
#12268=CARTESIAN_POINT('Ctrl Pts',(7.5,21.2953189477035,46.8862095951938));
#12269=CARTESIAN_POINT('Origin',(7.5,19.2953189477036,47.8862095951938));
#12270=CARTESIAN_POINT('Origin',(7.5,19.2953189477036,46.8862095951938));
#12271=CARTESIAN_POINT('Origin',(7.5,15.3987725179725,47.8862095951938));
#12272=CARTESIAN_POINT('Origin',(7.5,-6.43177298256785,47.8862095951938));
#12273=CARTESIAN_POINT('Ctrl Pts',(8.5,-7.43177298256785,46.8862095951938));
#12274=CARTESIAN_POINT('Ctrl Pts',(8.5,-7.43177298256785,47.8862095951938));
#12275=CARTESIAN_POINT('Ctrl Pts',(8.5,-6.43177298256785,47.8862095951938));
#12276=CARTESIAN_POINT('Ctrl Pts',(8.5,-8.43177298256784,46.8862095951938));
#12277=CARTESIAN_POINT('Ctrl Pts',(8.5,-8.43177298256784,48.8862095951938));
#12278=CARTESIAN_POINT('Ctrl Pts',(8.5,-6.43177298256785,48.8862095951938));
#12279=CARTESIAN_POINT('Ctrl Pts',(7.5,-8.43177298256784,46.8862095951938));
#12280=CARTESIAN_POINT('Ctrl Pts',(7.5,-8.43177298256784,48.8862095951938));
#12281=CARTESIAN_POINT('Ctrl Pts',(7.5,-6.43177298256785,48.8862095951938));
#12282=CARTESIAN_POINT('Origin',(7.5,-7.43177298256785,46.8862095951938));
#12283=CARTESIAN_POINT('Origin',(7.5,-6.43177298256785,46.8862095951938));
#12284=CARTESIAN_POINT('Origin',(7.5,-7.43177298256785,30.402562452839));
#12285=CARTESIAN_POINT('Origin',(7.5,-7.43177298256785,33.0483789742253));
#12286=CARTESIAN_POINT('Origin',(7.5,18.4692256236461,26.0483789742253));
#12287=CARTESIAN_POINT('',(7.5,26.4362251590507,27.0483789742253));
#12288=CARTESIAN_POINT('Origin',(7.5,26.4362251590507,26.0483789742253));
#12289=CARTESIAN_POINT('',(7.5,24.9477990585308,27.0483789742253));
#12290=CARTESIAN_POINT('',(7.5,18.4692256236461,27.0483789742253));
#12291=CARTESIAN_POINT('Origin',(7.5,24.9477990585308,26.0483789742253));
#12292=CARTESIAN_POINT('Origin',(7.5,24.9477990585308,29.5483789742253));
#12293=CARTESIAN_POINT('',(7.5,22.6973337979905,30.6371425441069));
#12294=CARTESIAN_POINT('Origin',(7.5,21.7971476937744,31.0726479720595));
#12295=CARTESIAN_POINT('Origin',(7.5,24.9477990585308,29.5483789742253));
#12296=CARTESIAN_POINT('Origin',(7.5,26.4362251590507,26.0483789742253));
#12297=CARTESIAN_POINT('Origin',(7.5,26.4362251590507,26.0483789742253));
#12298=CARTESIAN_POINT('Origin',(7.5,21.7971476937744,31.0726479720595));
#12299=CARTESIAN_POINT('Origin',(7.5,21.7971476937744,31.0726479720595));
#12300=CARTESIAN_POINT('Origin',(7.5,-7.43177298256785,33.0483789742253));
#12301=CARTESIAN_POINT('Origin',(7.5,-7.43177298256785,33.0483789742253));
#12302=CARTESIAN_POINT('Origin',(7.5,-7.43177298256785,26.0483789742253));
#12303=CARTESIAN_POINT('Origin',(7.5,-7.43177298256785,26.0483789742253));
#12304=CARTESIAN_POINT('Origin',(1.,-7.43177298256785,26.0483789742253));
#12305=CARTESIAN_POINT('',(2.5,-7.43177298256785,27.0483789742253));
#12306=CARTESIAN_POINT('',(1.,-7.43177298256785,27.0483789742253));
#12307=CARTESIAN_POINT('Origin',(2.5,-7.43177298256785,26.0483789742253));
#12308=CARTESIAN_POINT('Origin',(8.5,-5.94334688204796,27.0483789742253));
#12309=CARTESIAN_POINT('',(2.5,-5.94334688204796,27.0483789742253));
#12310=CARTESIAN_POINT('',(8.5,-5.94334688204796,27.0483789742253));
#12311=CARTESIAN_POINT('',(2.5,-5.94334688204796,27.0483789742253));
#12312=CARTESIAN_POINT('Origin',(8.5,-5.94334688204796,29.5483789742253));
#12313=CARTESIAN_POINT('',(2.5,-5.94334688204796,32.0483789742253));
#12314=CARTESIAN_POINT('',(8.5,-5.94334688204796,32.0483789742253));
#12315=CARTESIAN_POINT('Origin',(2.5,-5.94334688204796,29.5483789742253));
#12316=CARTESIAN_POINT('Origin',(8.5,-8.43177298256785,32.0483789742253));
#12317=CARTESIAN_POINT('',(2.5,-7.43177298256785,32.0483789742253));
#12318=CARTESIAN_POINT('',(1.,-7.43177298256785,32.0483789742253));
#12319=CARTESIAN_POINT('',(2.5,-5.94334688204796,32.0483789742253));
#12320=CARTESIAN_POINT('Origin',(1.,-7.43177298256785,33.0483789742253));
#12321=CARTESIAN_POINT('Origin',(2.5,-7.43177298256785,33.0483789742253));
#12322=CARTESIAN_POINT('Origin',(-6.5,-6.43177298256785,46.8862095951938));
#12323=CARTESIAN_POINT('Origin',(-6.5,19.2953189477036,46.8862095951938));
#12324=CARTESIAN_POINT('',(-6.5,21.2953189477036,46.8862095951938));
#12325=CARTESIAN_POINT('Origin',(-6.5,21.2953189477036,33.0096109045284));
#12326=CARTESIAN_POINT('',(-6.5,21.2953189477036,33.0096109045284));
#12327=CARTESIAN_POINT('Origin',(-6.5,22.2953189477035,33.0096109045284));
#12328=CARTESIAN_POINT('',(2.5,22.046233320739,32.041129438294));
#12329=CARTESIAN_POINT('',(-6.5,22.046233320739,32.041129438294));
#12330=CARTESIAN_POINT('',(2.5,22.2953189477036,32.0096109045284));
#12331=CARTESIAN_POINT('Origin',(2.5,22.2953189477035,33.0096109045284));
#12332=CARTESIAN_POINT('',(-6.5,22.2953189477036,32.0096109045284));
#12333=CARTESIAN_POINT('Origin',(-6.5,21.7971476937744,31.0726479720595));
#12334=CARTESIAN_POINT('',(2.5,22.6973337979905,30.6371425441069));
#12335=CARTESIAN_POINT('',(-6.5,22.6973337979905,30.6371425441069));
#12336=CARTESIAN_POINT('Origin',(2.5,21.7971476937744,31.0726479720595));
#12337=CARTESIAN_POINT('Origin',(8.5,24.9477990585308,29.5483789742253));
#12338=CARTESIAN_POINT('',(2.5,24.9477990585308,27.0483789742253));
#12339=CARTESIAN_POINT('',(8.5,24.9477990585308,27.0483789742253));
#12340=CARTESIAN_POINT('Origin',(2.5,24.9477990585308,29.5483789742253));
#12341=CARTESIAN_POINT('Origin',(8.5,27.4362251590507,27.0483789742253));
#12342=CARTESIAN_POINT('',(2.5,26.4362251590507,27.0483789742253));
#12343=CARTESIAN_POINT('',(1.,26.4362251590507,27.0483789742253));
#12344=CARTESIAN_POINT('',(2.5,24.9477990585308,27.0483789742253));
#12345=CARTESIAN_POINT('Origin',(1.,26.4362251590507,26.0483789742253));
#12346=CARTESIAN_POINT('Origin',(2.5,26.4362251590507,26.0483789742253));
#12347=CARTESIAN_POINT('Origin',(8.5,-8.43177298256785,-19.9105093470644));
#12348=CARTESIAN_POINT('',(2.5,-6.00539963551477,-19.9105093470644));
#12349=CARTESIAN_POINT('',(2.5,-6.00539963551477,-19.9105093470644));
#12350=CARTESIAN_POINT('',(8.5,-6.00539963551477,-19.9105093470644));
#12351=CARTESIAN_POINT('Origin',(8.5,-3.50539963551477,-22.4105093470644));
#12352=CARTESIAN_POINT('',(2.5,-3.50539963551477,-22.4105093470644));
#12353=CARTESIAN_POINT('',(8.5,-3.50539963551477,-22.4105093470644));
#12354=CARTESIAN_POINT('',(2.5,-3.50539963551477,-25.0483789742253));
#12355=CARTESIAN_POINT('',(2.5,-3.50539963551477,-22.4105093470644));
#12356=CARTESIAN_POINT('',(1.,-3.50539963551477,-25.0483789742253));
#12357=CARTESIAN_POINT('Origin',(8.5,-6.00539963551477,-22.4105093470644));
#12358=CARTESIAN_POINT('Origin',(2.5,-6.00539963551477,-22.4105093470644));
#12359=CARTESIAN_POINT('Origin',(2.5,-5.96858630904131,-22.4794441606449));
#12360=CARTESIAN_POINT('',(2.5,-6.43177298256785,-25.0483789742253));
#12361=CARTESIAN_POINT('Origin',(2.5,-6.43177298256785,-23.0483789742253));
#12362=CARTESIAN_POINT('',(2.5,-6.20017964580458,-25.0483789742253));
#12363=CARTESIAN_POINT('Origin',(2.5,24.9420121087908,29.5289949393769));
#12364=CARTESIAN_POINT('',(2.5,25.4362251590507,32.0096109045284));
#12365=CARTESIAN_POINT('',(2.5,25.1891186339208,32.0096109045284));
#12366=CARTESIAN_POINT('Origin',(2.5,25.4362251590507,30.0096109045284));
#12367=CARTESIAN_POINT('Origin',(8.5,25.0098518119976,-19.9105093470644));
#12368=CARTESIAN_POINT('',(2.5,25.0098518119976,-19.9105093470644));
#12369=CARTESIAN_POINT('',(8.5,25.0098518119976,-19.9105093470644));
#12370=CARTESIAN_POINT('',(2.5,25.0098518119976,-19.9105093470644));
#12371=CARTESIAN_POINT('Origin',(8.5,25.0098518119976,-22.4105093470644));
#12372=CARTESIAN_POINT('',(2.5,22.5098518119976,-22.4105093470644));
#12373=CARTESIAN_POINT('',(8.5,22.5098518119976,-22.4105093470644));
#12374=CARTESIAN_POINT('Origin',(2.5,25.0098518119976,-22.4105093470644));
#12375=CARTESIAN_POINT('Origin',(8.5,22.5098518119976,-25.0483789742253));
#12376=CARTESIAN_POINT('',(2.5,22.5098518119976,-25.0483789742253));
#12377=CARTESIAN_POINT('',(1.,22.5098518119976,-25.0483789742253));
#12378=CARTESIAN_POINT('',(2.5,22.5098518119976,-22.4105093470644));
#12379=CARTESIAN_POINT('Origin',(2.5,24.9730384855242,-22.4794441606449));
#12380=CARTESIAN_POINT('',(2.5,25.4362251590507,-25.0483789742253));
#12381=CARTESIAN_POINT('',(2.5,9.27063275147817,-25.0483789742253));
#12382=CARTESIAN_POINT('Origin',(2.5,25.4362251590507,-23.0483789742253));
#12383=CARTESIAN_POINT('Origin',(2.5,-5.93755993230791,29.5483789742253));
#12384=CARTESIAN_POINT('Origin',(-6.5,25.4362251590507,32.0096109045284));
#12385=CARTESIAN_POINT('',(-6.5,25.4362251590507,32.0096109045284));
#12386=CARTESIAN_POINT('Origin',(-6.5,-6.43177298256785,-25.0483789742253));
#12387=CARTESIAN_POINT('',(-6.5,25.4362251590507,-25.0483789742253));
#12388=CARTESIAN_POINT('',(-6.5,-6.43177298256785,-25.0483789742253));
#12389=CARTESIAN_POINT('Origin',(-6.5,25.4362251590507,30.0096109045284));
#12390=CARTESIAN_POINT('Origin',(-6.5,25.4362251590507,-23.0483789742253));
#12391=CARTESIAN_POINT('Origin',(-6.5,-6.43177298256785,-23.0483789742253));
#12392=CARTESIAN_POINT('',(0.,0.,0.));
#12393=CARTESIAN_POINT('Origin',(-0.499999999999999,9.50222608824143,11.9189153104842));
#12394=CARTESIAN_POINT('',(-0.499999999999999,22.2688065021356,-20.2341199955735));
#12395=CARTESIAN_POINT('',(-0.5,22.2688065021356,-25.0483789742253));
#12396=CARTESIAN_POINT('',(-0.499999999999999,22.2688065021356,-6.56473183187052));
#12397=CARTESIAN_POINT('',(-0.499999999999999,25.4362251590507,-25.0483789742253));
#12398=CARTESIAN_POINT('',(-0.499999999999999,25.4362251590507,-25.0483789742253));
#12399=CARTESIAN_POINT('',(-0.499999999999999,27.4362251590507,-23.0483789742253));
#12400=CARTESIAN_POINT('Origin',(-0.499999999999999,25.4362251590507,-23.0483789742253));
#12401=CARTESIAN_POINT('',(-0.499999999999999,27.4362251590507,30.0096109045284));
#12402=CARTESIAN_POINT('',(-0.499999999999999,27.4362251590507,30.0096109045284));
#12403=CARTESIAN_POINT('',(-0.499999999999999,25.4362251590507,32.0096109045284));
#12404=CARTESIAN_POINT('Origin',(-0.499999999999999,25.4362251590507,30.0096109045284));
#12405=CARTESIAN_POINT('',(-0.499999999999999,22.2953189477036,32.0096109045284));
#12406=CARTESIAN_POINT('',(-0.499999999999999,22.2953189477036,32.0096109045284));
#12407=CARTESIAN_POINT('',(-0.499999999999999,21.2953189477036,33.0096109045284));
#12408=CARTESIAN_POINT('Origin',(-0.499999999999999,22.2953189477035,33.0096109045284));
#12409=CARTESIAN_POINT('',(-0.499999999999999,21.2953189477036,46.8862095951938));
#12410=CARTESIAN_POINT('',(-0.499999999999999,21.2953189477036,46.8862095951938));
#12411=CARTESIAN_POINT('',(-0.499999999999999,19.2953189477036,48.8862095951938));
#12412=CARTESIAN_POINT('Origin',(-0.499999999999999,19.2953189477036,46.8862095951938));
#12413=CARTESIAN_POINT('',(-0.499999999999999,18.4317729825679,48.8862095951938));
#12414=CARTESIAN_POINT('',(-0.499999999999999,-6.43177298256785,48.8862095951938));
#12415=CARTESIAN_POINT('',(-0.499999999999999,18.4317729825679,46.8862095951938));
#12416=CARTESIAN_POINT('',(-0.499999999999999,18.4317729825679,30.402562452839));
#12417=CARTESIAN_POINT('',(-0.499999999999999,19.2953189477036,46.8862095951938));
#12418=CARTESIAN_POINT('',(-0.499999999999999,1.53522655283679,46.8862095951938));
#12419=CARTESIAN_POINT('',(-0.499999999999999,19.2953189477036,33.0096109045284));
#12420=CARTESIAN_POINT('',(-0.499999999999999,19.2953189477035,29.402562452839));
#12421=CARTESIAN_POINT('',(-0.499999999999999,21.4945386978003,30.1184604429708));
#12422=CARTESIAN_POINT('Origin',(-0.499999999999999,22.2953189477035,33.0096109045284));
#12423=CARTESIAN_POINT('',(-0.499999999999999,25.4362251590507,26.0826265387027));
#12424=CARTESIAN_POINT('Origin',(-0.499999999999999,24.9477990585308,29.5483789742253));
#12425=CARTESIAN_POINT('',(-0.499999999999999,25.4362251590507,-18.9365770263474));
#12426=CARTESIAN_POINT('',(-0.499999999999999,25.4362251590507,20.9642631075063));
#12427=CARTESIAN_POINT('Origin',(-0.499999999999999,25.0098518119976,-22.4105093470644));
#12428=CARTESIAN_POINT('',(-0.499999999999999,23.4477990585308,29.5483789742253));
#12429=CARTESIAN_POINT('Origin',(-0.499999999999999,24.9477990585308,29.5483789742253));
#12430=CARTESIAN_POINT('',(-0.499999999999999,23.5098518119976,-22.4105093470644));
#12431=CARTESIAN_POINT('Origin',(-0.499999999999999,25.0098518119976,-22.4105093470644));
#12432=CARTESIAN_POINT('Ctrl Pts',(-13.112465101899,-4.10380624392837,-40.0483789742253));
#12433=CARTESIAN_POINT('Ctrl Pts',(-15.112465101899,-4.10380624392837,-40.0483789742253));
#12434=CARTESIAN_POINT('Ctrl Pts',(-15.112465101899,-2.10380624392837,-40.0483789742253));
#12435=CARTESIAN_POINT('Ctrl Pts',(-13.112465101899,-4.10380624392837,-41.0483789742253));
#12436=CARTESIAN_POINT('Ctrl Pts',(-15.112465101899,-4.10380624392837,-41.0483789742253));
#12437=CARTESIAN_POINT('Ctrl Pts',(-15.112465101899,-2.10380624392837,-41.0483789742253));
#12438=CARTESIAN_POINT('Ctrl Pts',(-13.112465101899,-3.10380624392837,-41.0483789742253));
#12439=CARTESIAN_POINT('Ctrl Pts',(-14.112465101899,-3.10380624392837,-41.0483789742253));
#12440=CARTESIAN_POINT('Ctrl Pts',(-14.112465101899,-2.10380624392837,-41.0483789742253));
#12441=CARTESIAN_POINT('',(-13.112465101899,-3.10380624392837,-41.0483789742253));
#12442=CARTESIAN_POINT('',(-13.112465101899,-4.10380624392837,-40.0483789742253));
#12443=CARTESIAN_POINT('Origin',(-13.112465101899,-3.10380624392837,-40.0483789742253));
#12444=CARTESIAN_POINT('',(-15.112465101899,-2.10380624392837,-40.0483789742253));
#12445=CARTESIAN_POINT('Origin',(-13.112465101899,-2.10380624392837,-40.0483789742253));
#12446=CARTESIAN_POINT('',(-14.112465101899,-2.10380624392837,-41.0483789742253));
#12447=CARTESIAN_POINT('Origin',(-14.112465101899,-2.10380624392837,-40.0483789742253));
#12448=CARTESIAN_POINT('Origin',(-13.112465101899,-2.10380624392837,-41.0483789742253));
#12449=CARTESIAN_POINT('Origin',(-5.56259599847326,-3.10380624392837,-40.0483789742253));
#12450=CARTESIAN_POINT('',(-2.49997296399801,-3.10380624392837,-41.0483789742253));
#12451=CARTESIAN_POINT('',(-2.49997296399801,-4.10380624392837,-40.0483789742253));
#12452=CARTESIAN_POINT('Origin',(-2.49997296399801,-3.10380624392837,-40.0483789742253));
#12453=CARTESIAN_POINT('',(-5.56259599847326,-4.10380624392837,-40.0483789742253));
#12454=CARTESIAN_POINT('',(-5.56259599847326,-3.10380624392837,-41.0483789742253));
#12455=CARTESIAN_POINT('Ctrl Pts',(-15.112465101899,14.8031072225088,-40.0483789742253));
#12456=CARTESIAN_POINT('Ctrl Pts',(-15.112465101899,16.8031072225088,-40.0483789742253));
#12457=CARTESIAN_POINT('Ctrl Pts',(-13.112465101899,16.8031072225088,-40.0483789742253));
#12458=CARTESIAN_POINT('Ctrl Pts',(-15.112465101899,14.8031072225088,-41.0483789742253));
#12459=CARTESIAN_POINT('Ctrl Pts',(-15.112465101899,16.8031072225088,-41.0483789742253));
#12460=CARTESIAN_POINT('Ctrl Pts',(-13.112465101899,16.8031072225088,-41.0483789742253));
#12461=CARTESIAN_POINT('Ctrl Pts',(-14.112465101899,14.8031072225088,-41.0483789742253));
#12462=CARTESIAN_POINT('Ctrl Pts',(-14.112465101899,15.8031072225088,-41.0483789742253));
#12463=CARTESIAN_POINT('Ctrl Pts',(-13.112465101899,15.8031072225088,-41.0483789742253));
#12464=CARTESIAN_POINT('',(-14.112465101899,14.8031072225088,-41.0483789742253));
#12465=CARTESIAN_POINT('',(-15.112465101899,14.8031072225088,-40.0483789742253));
#12466=CARTESIAN_POINT('Origin',(-14.112465101899,14.8031072225088,-40.0483789742253));
#12467=CARTESIAN_POINT('',(-13.112465101899,16.8031072225088,-40.0483789742253));
#12468=CARTESIAN_POINT('Origin',(-13.112465101899,14.8031072225088,-40.0483789742253));
#12469=CARTESIAN_POINT('',(-13.112465101899,15.8031072225088,-41.0483789742253));
#12470=CARTESIAN_POINT('Origin',(-13.112465101899,15.8031072225088,-40.0483789742253));
#12471=CARTESIAN_POINT('Origin',(-13.112465101899,14.8031072225088,-41.0483789742253));
#12472=CARTESIAN_POINT('Origin',(-11.4097522506131,15.8031073387245,-40.0483789742253));
#12473=CARTESIAN_POINT('',(-1.49997296399801,15.8031073387245,-41.0483789742253));
#12474=CARTESIAN_POINT('',(-11.4097522506131,15.8031073387245,-41.0483789742253));
#12475=CARTESIAN_POINT('',(-0.499972963998009,16.8031073387245,-40.0483789742253));
#12476=CARTESIAN_POINT('',(-11.4097522506131,16.8031073387245,-40.0483789742253));
#12477=CARTESIAN_POINT('Origin',(-1.49997296399801,15.8031073387245,-40.0483789742253));
#12478=CARTESIAN_POINT('Origin',(-1.49997296399801,10.5763788558995,-40.0483789742253));
#12479=CARTESIAN_POINT('',(-0.499972963998009,-2.10380624392837,-40.0483789742253));
#12480=CARTESIAN_POINT('',(-0.499972963998009,10.5763788558995,-40.0483789742253));
#12481=CARTESIAN_POINT('',(-1.49997296399801,-2.10380624392837,-41.0483789742253));
#12482=CARTESIAN_POINT('Origin',(-1.49997296399801,-2.10380624392837,-40.0483789742253));
#12483=CARTESIAN_POINT('',(-1.49997296399801,10.5763788558995,-41.0483789742253));
#12484=CARTESIAN_POINT('Ctrl Pts',(-2.49997296399801,-3.10380624392837,
-41.0483789742253));
#12485=CARTESIAN_POINT('Ctrl Pts',(-1.49997296399801,-3.10380624392837,
-41.0483789742253));
#12486=CARTESIAN_POINT('Ctrl Pts',(-1.49997296399801,-2.10380624392837,
-41.0483789742253));
#12487=CARTESIAN_POINT('Ctrl Pts',(-2.49997296399801,-4.10380624392837,
-41.0483789742253));
#12488=CARTESIAN_POINT('Ctrl Pts',(-0.499972963998009,-4.10380624392837,
-41.0483789742253));
#12489=CARTESIAN_POINT('Ctrl Pts',(-0.499972963998009,-2.10380624392837,
-41.0483789742253));
#12490=CARTESIAN_POINT('Ctrl Pts',(-2.49997296399801,-4.10380624392837,
-40.0483789742253));
#12491=CARTESIAN_POINT('Ctrl Pts',(-0.499972963998009,-4.10380624392837,
-40.0483789742253));
#12492=CARTESIAN_POINT('Ctrl Pts',(-0.499972963998009,-2.10380624392837,
-40.0483789742253));
#12493=CARTESIAN_POINT('Origin',(-2.49997296399801,-2.10380624392837,-40.0483789742253));
#12494=CARTESIAN_POINT('Origin',(-2.49997296399801,-2.10380624392837,-41.0483789742253));
#12495=CARTESIAN_POINT('Origin',(-13.112465101899,-2.10380624392837,-25.0483789742253));
#12496=CARTESIAN_POINT('',(-13.112465101899,-4.10380624392837,-25.0483789742253));
#12497=CARTESIAN_POINT('',(-13.112465101899,-4.10380624392837,-25.0483789742253));
#12498=CARTESIAN_POINT('',(-15.112465101899,-2.10380624392837,-25.0483789742253));
#12499=CARTESIAN_POINT('Origin',(-13.112465101899,-2.10380624392837,-25.0483789742253));
#12500=CARTESIAN_POINT('',(-15.112465101899,-2.10380624392837,-25.0483789742253));
#12501=CARTESIAN_POINT('Origin',(-3.04597296399801,-4.10380624392837,-25.0483789742253));
#12502=CARTESIAN_POINT('',(-2.49997296399801,-4.10380624392837,-25.0483789742253));
#12503=CARTESIAN_POINT('',(-2.49997296399801,-4.10380624392837,-25.0483789742253));
#12504=CARTESIAN_POINT('',(-1.772986481999,-4.10380624392837,-25.0483789742253));
#12505=CARTESIAN_POINT('Origin',(-2.49997296399801,-2.10380624392837,-25.0483789742253));
#12506=CARTESIAN_POINT('',(-0.499999999999999,-2.10380624392837,-25.0483789742253));
#12507=CARTESIAN_POINT('',(-0.499972963998009,-2.10380624392837,-25.0483789742253));
#12508=CARTESIAN_POINT('',(-0.499999999999999,-2.11420543990764,-25.0483789742253));
#12509=CARTESIAN_POINT('',(-0.499999999999999,25.4362251590507,-25.0483789742253));
#12510=CARTESIAN_POINT('Origin',(-2.49997296399801,-2.10380624392837,-25.0483789742253));
#12511=CARTESIAN_POINT('Origin',(-0.499972963998009,14.8031072225088,-25.0483789742253));
#12512=CARTESIAN_POINT('',(-0.499999999999999,16.8031073387245,-25.0483789742253));
#12513=CARTESIAN_POINT('',(-0.499972963998009,16.8031073387245,-25.0483789742253));
#12514=CARTESIAN_POINT('',(-0.499999999999999,25.4362251590507,-25.0483789742253));
#12515=CARTESIAN_POINT('',(-0.499972963998008,10.4317729825678,-32.9865355928432));
#12516=CARTESIAN_POINT('Origin',(-0.499972963998008,6.43177298256785,-32.9865355928432));
#12517=CARTESIAN_POINT('Origin',(-14.7402854682776,16.8031073387245,-25.0483789742253));
#12518=CARTESIAN_POINT('',(-13.112465101899,16.8031072225088,-25.0483789742253));
#12519=CARTESIAN_POINT('',(-13.112465101899,16.8031072225088,-25.0483789742253));
#12520=CARTESIAN_POINT('',(-14.7402854682776,16.8031073387245,-25.0483789742253));
#12521=CARTESIAN_POINT('',(-7.62014273413882,16.8031073387245,-25.0483789742253));
#12522=CARTESIAN_POINT('',(-14.7402854682776,16.8031073387245,-23.0483789742253));
#12523=CARTESIAN_POINT('',(-14.7402854682776,16.8031073387245,-25.0483789742253));
#12524=CARTESIAN_POINT('',(-0.499999999999999,16.8031073387245,-23.0483789742253));
#12525=CARTESIAN_POINT('',(-7.62014273413882,16.8031073387245,-23.0483789742253));
#12526=CARTESIAN_POINT('',(-0.499999999999999,16.8031073387245,-6.56473183187052));
#12527=CARTESIAN_POINT('Origin',(-14.112465101899,2.12292212268092,-40.0483789742253));
#12528=CARTESIAN_POINT('',(-15.112465101899,2.12292212268092,-40.0483789742253));
#12529=CARTESIAN_POINT('',(-14.112465101899,2.12292212268092,-41.0483789742253));
#12530=CARTESIAN_POINT('Origin',(-13.112465101899,14.8031072225088,-25.0483789742253));
#12531=CARTESIAN_POINT('',(-15.112465101899,14.8031072225088,-25.0483789742253));
#12532=CARTESIAN_POINT('',(-15.112465101899,14.8031072225088,-25.0483789742253));
#12533=CARTESIAN_POINT('Origin',(-13.112465101899,14.8031072225088,-25.0483789742253));
#12534=CARTESIAN_POINT('Origin',(-8.07921903294852,6.34965048929021,-41.0483789742253));
#12535=CARTESIAN_POINT('Origin',(-0.499999999999999,25.4362251590507,-25.0483789742253));
#12536=CARTESIAN_POINT('',(-0.499999999999999,-6.43177298256785,-25.0483789742253));
#12537=CARTESIAN_POINT('',(-0.499999999999999,25.4362251590507,-25.0483789742253));
#12538=CARTESIAN_POINT('',(-20.5,-6.43177298256785,-25.0483789742253));
#12539=CARTESIAN_POINT('',(-0.499999999999999,-6.43177298256785,-25.0483789742253));
#12540=CARTESIAN_POINT('',(-20.5,25.4362251590507,-25.0483789742253));
#12541=CARTESIAN_POINT('',(-20.5,17.4692256236461,-25.0483789742253));
#12542=CARTESIAN_POINT('',(-0.499999999999999,25.4362251590507,-25.0483789742253));
#12543=CARTESIAN_POINT('',(-14.7402854682776,22.2688065021356,-25.0483789742253));
#12544=CARTESIAN_POINT('',(0.620142734138823,22.2688065021356,-25.0483789742253));
#12545=CARTESIAN_POINT('',(-15.7402854682776,21.2688065021356,-25.0483789742253));
#12546=CARTESIAN_POINT('Origin',(-14.7402854682776,21.2688065021356,-25.0483789742253));
#12547=CARTESIAN_POINT('',(-15.7402854682776,17.8031073387245,-25.0483789742253));
#12548=CARTESIAN_POINT('',(-15.7402854682776,23.3525158305932,-25.0483789742253));
#12549=CARTESIAN_POINT('Origin',(-14.7402854682776,17.8031073387245,-25.0483789742253));
#12550=CARTESIAN_POINT('',(-15.112465101899,11.6662094575612,-25.0483789742253));
#12551=CARTESIAN_POINT('Origin',(-15.112465101899,6.43177298256785,-32.9865355928432));
#12552=CARTESIAN_POINT('',(-15.112465101899,10.4317729825678,-32.9865355928432));
#12553=CARTESIAN_POINT('Origin',(-15.112465101899,6.43177298256785,-32.9865355928432));
#12554=CARTESIAN_POINT('',(-15.112465101899,10.4317729825678,-32.9865355928432));
#12555=CARTESIAN_POINT('Origin',(-15.112465101899,-2.10380624392837,-25.0483789742253));
#12556=CARTESIAN_POINT('Origin',(1.74028546827764,22.2688065021356,-25.0483789742253));
#12557=CARTESIAN_POINT('',(-14.7402854682776,22.2688065021356,-20.2341199955735));
#12558=CARTESIAN_POINT('',(-0.499999999999999,22.2688065021356,-20.2341199955735));
#12559=CARTESIAN_POINT('',(-14.7402854682776,22.2688065021356,-25.0483789742253));
#12560=CARTESIAN_POINT('Origin',(-15.7402854682776,21.2688065021356,-25.0483789742253));
#12561=CARTESIAN_POINT('',(-15.7402854682776,21.2688065021356,-23.0483789742253));
#12562=CARTESIAN_POINT('',(-15.7402854682776,21.2688065021356,-25.0483789742253));
#12563=CARTESIAN_POINT('',(-15.7402854682776,17.8031073387245,-23.0483789742253));
#12564=CARTESIAN_POINT('',(-15.7402854682776,23.3525158305932,-23.0483789742253));
#12565=CARTESIAN_POINT('',(-15.7402854682776,17.8031073387245,-25.0483789742253));
#12566=CARTESIAN_POINT('Origin',(-14.7402854682776,21.2688065021356,-25.0483789742253));
#12567=CARTESIAN_POINT('',(-15.694331048449,21.5684680294553,-23.0483789742253));
#12568=CARTESIAN_POINT('Ctrl Pts',(-15.694331048449,21.5684680294553,-23.0483789742253));
#12569=CARTESIAN_POINT('Ctrl Pts',(-15.7067045333496,21.5290740215346,-22.8358435371785));
#12570=CARTESIAN_POINT('Ctrl Pts',(-15.7107993314416,21.5098518119976,-22.6191838880156));
#12571=CARTESIAN_POINT('Ctrl Pts',(-15.7107993314416,21.5098518119976,-22.0465473119767));
#12572=CARTESIAN_POINT('Ctrl Pts',(-15.7017461665905,21.5718168405896,-21.6587360262855));
#12573=CARTESIAN_POINT('Ctrl Pts',(-15.6217540845814,21.7453252007984,-21.1350970538315));
#12574=CARTESIAN_POINT('Ctrl Pts',(-15.5832369350269,21.8154399994892,-20.9705071584932));
#12575=CARTESIAN_POINT('Ctrl Pts',(-15.4627032474283,21.9670099916972,-20.6729862218086));
#12576=CARTESIAN_POINT('Ctrl Pts',(-15.3825634860813,22.048920053459,-20.5395299428976));
#12577=CARTESIAN_POINT('Ctrl Pts',(-15.1938793645158,22.1631936845831,-20.3730368907704));
#12578=CARTESIAN_POINT('Ctrl Pts',(-15.1132023218396,22.201380934103,-20.3213948743704));
#12579=CARTESIAN_POINT('Ctrl Pts',(-14.9336495994831,22.2543889579894,-20.2519607649698));
#12580=CARTESIAN_POINT('Ctrl Pts',(-14.8346739441802,22.2688065021356,-20.2341199955735));
#12581=CARTESIAN_POINT('Ctrl Pts',(-14.7402854682776,22.2688065021356,-20.2341199955735));
#12582=CARTESIAN_POINT('Origin',(-14.7402854682776,21.2688065021356,-23.0483789742253));
#12583=CARTESIAN_POINT('Origin',(-14.7402854682776,17.8031073387245,-25.0483789742253));
#12584=CARTESIAN_POINT('Origin',(-14.7402854682776,17.8031073387245,-23.0483789742253));
#12585=CARTESIAN_POINT('Origin',(-0.499999999999999,9.50222608824143,11.9189153104842));
#12586=CARTESIAN_POINT('',(-0.499999999999999,-2.56401585297239,-23.0483789742253));
#12587=CARTESIAN_POINT('',(-0.499999999999999,17.4692256236461,-23.0483789742253));
#12588=CARTESIAN_POINT('',(-0.499999999999999,-6.43177298256785,-18.9365770263474));
#12589=CARTESIAN_POINT('Origin',(-0.499999999999999,-6.00539963551477,-22.4105093470644));
#12590=CARTESIAN_POINT('',(-0.499999999999999,-6.43177298256785,26.0826265387027));
#12591=CARTESIAN_POINT('',(-0.499999999999999,-6.43177298256785,-5.56473183187052));
#12592=CARTESIAN_POINT('',(-0.499999999999999,-6.43177298256785,33.0141314097479));
#12593=CARTESIAN_POINT('Origin',(-0.499999999999999,-5.94334688204796,29.5483789742253));
#12594=CARTESIAN_POINT('',(-0.499999999999999,-6.43177298256785,46.8862095951938));
#12595=CARTESIAN_POINT('',(-0.499999999999999,-6.43177298256785,-5.56473183187052));
#12596=CARTESIAN_POINT('',(-0.499999999999999,-5.56822701743215,46.8862095951938));
#12597=CARTESIAN_POINT('',(-0.499999999999999,1.53522655283679,46.8862095951938));
#12598=CARTESIAN_POINT('',(-0.499999999999999,-5.56822701743215,48.8862095951938));
#12599=CARTESIAN_POINT('',(-0.499999999999999,-5.56822701743215,30.402562452839));
#12600=CARTESIAN_POINT('',(-0.499999999999999,-6.43177298256785,48.8862095951938));
#12601=CARTESIAN_POINT('',(-0.499999999999999,-6.43177298256785,48.8862095951938));
#12602=CARTESIAN_POINT('',(-0.499999999999999,-8.43177298256785,46.8862095951938));
#12603=CARTESIAN_POINT('Origin',(-0.499999999999999,-6.43177298256785,46.8862095951938));
#12604=CARTESIAN_POINT('',(-0.499999999999999,-8.43177298256785,-23.0483789742253));
#12605=CARTESIAN_POINT('',(-0.499999999999999,-8.43177298256785,-23.0483789742253));
#12606=CARTESIAN_POINT('Origin',(-0.499999999999999,-6.43177298256785,-23.0483789742253));
#12607=CARTESIAN_POINT('',(-0.499999999999999,-7.44334688204796,29.5483789742253));
#12608=CARTESIAN_POINT('Origin',(-0.499999999999999,-5.94334688204796,29.5483789742253));
#12609=CARTESIAN_POINT('',(-0.499999999999999,-7.50539963551477,-22.4105093470644));
#12610=CARTESIAN_POINT('Origin',(-0.499999999999999,-6.00539963551477,-22.4105093470644));
#12611=CARTESIAN_POINT('Origin',(-16.5,-3.56822701743215,48.8862095951938));
#12612=CARTESIAN_POINT('',(-18.5,-3.56822701743215,46.8862095951938));
#12613=CARTESIAN_POINT('',(-16.5,-5.56822701743215,46.8862095951938));
#12614=CARTESIAN_POINT('Origin',(-16.5,-3.56822701743215,46.8862095951938));
#12615=CARTESIAN_POINT('',(-18.5,-3.56822701743215,48.8862095951938));
#12616=CARTESIAN_POINT('',(-18.5,-3.56822701743215,48.8862095951938));
#12617=CARTESIAN_POINT('',(-16.5,-5.56822701743215,48.8862095951938));
#12618=CARTESIAN_POINT('Origin',(-16.5,-3.56822701743215,48.8862095951938));
#12619=CARTESIAN_POINT('',(-16.5,-5.56822701743215,48.8862095951938));
#12620=CARTESIAN_POINT('Origin',(3.5,-5.56822701743215,48.8862095951938));
#12621=CARTESIAN_POINT('',(1.5,-5.56822701743215,46.8862095951938));
#12622=CARTESIAN_POINT('',(1.5,-5.56822701743215,48.8862095951938));
#12623=CARTESIAN_POINT('Origin',(-16.5,18.4317729825679,48.8862095951938));
#12624=CARTESIAN_POINT('',(-16.5,18.4317729825679,46.8862095951938));
#12625=CARTESIAN_POINT('',(-8.5,18.4317729825679,46.8862095951938));
#12626=CARTESIAN_POINT('',(-16.5,18.4317729825679,48.8862095951938));
#12627=CARTESIAN_POINT('',(-8.5,18.4317729825679,48.8862095951938));
#12628=CARTESIAN_POINT('',(-16.5,18.4317729825679,48.8862095951938));
#12629=CARTESIAN_POINT('Origin',(-16.5,16.4317729825679,48.8862095951938));
#12630=CARTESIAN_POINT('',(-18.5,16.4317729825679,46.8862095951938));
#12631=CARTESIAN_POINT('Origin',(-16.5,16.4317729825679,46.8862095951938));
#12632=CARTESIAN_POINT('',(-18.5,16.4317729825679,48.8862095951938));
#12633=CARTESIAN_POINT('Origin',(-16.5,16.4317729825679,48.8862095951938));
#12634=CARTESIAN_POINT('',(-18.5,16.4317729825679,48.8862095951938));
#12635=CARTESIAN_POINT('Origin',(-18.5,-3.56822701743215,48.8862095951938));
#12636=CARTESIAN_POINT('',(-18.5,-5.,46.8862095951938));
#12637=CARTESIAN_POINT('',(-18.5,-5.,48.8862095951938));
#12638=CARTESIAN_POINT('Origin',(-0.499999999999999,-6.43177298256785,48.8862095951938));
#12639=CARTESIAN_POINT('',(-20.5,19.2953189477036,48.8862095951938));
#12640=CARTESIAN_POINT('',(-0.499999999999999,19.2953189477036,48.8862095951938));
#12641=CARTESIAN_POINT('',(-20.5,-6.43177298256785,48.8862095951938));
#12642=CARTESIAN_POINT('',(-20.5,1.53522655283679,48.8862095951938));
#12643=CARTESIAN_POINT('',(-0.499999999999999,-6.43177298256785,48.8862095951938));
#12644=CARTESIAN_POINT('Origin',(-0.499999999999999,25.4362251590507,-23.0483789742253));
#12645=CARTESIAN_POINT('',(-19.5,21.5684680294553,-23.0483789742253));
#12646=CARTESIAN_POINT('',(-0.499999999999999,21.5684680294553,-23.0483789742253));
#12647=CARTESIAN_POINT('',(-19.5,-2.56401585297239,-23.0483789742253));
#12648=CARTESIAN_POINT('',(-19.5,17.4692256236461,-23.0483789742253));
#12649=CARTESIAN_POINT('',(-0.499999999999999,-2.56401585297239,-23.0483789742253));
#12650=CARTESIAN_POINT('Origin',(-19.5,9.50222608824143,11.9189153104842));
#12651=CARTESIAN_POINT('',(-19.5,25.4362251590507,-18.9365770263474));
#12652=CARTESIAN_POINT('Origin',(-19.5,25.0098518119976,-22.4105093470644));
#12653=CARTESIAN_POINT('',(-19.5,25.4362251590507,26.0826265387027));
#12654=CARTESIAN_POINT('',(-19.5,25.4362251590507,20.9642631075063));
#12655=CARTESIAN_POINT('',(-19.5,21.4945386978003,30.1184604429708));
#12656=CARTESIAN_POINT('Origin',(-19.5,24.9477990585308,29.5483789742253));
#12657=CARTESIAN_POINT('',(-19.5,19.2953189477036,33.0096109045284));
#12658=CARTESIAN_POINT('Origin',(-19.5,22.2953189477035,33.0096109045284));
#12659=CARTESIAN_POINT('',(-19.5,19.2953189477036,46.8862095951938));
#12660=CARTESIAN_POINT('',(-19.5,19.2953189477035,29.402562452839));
#12661=CARTESIAN_POINT('',(-19.5,-6.43177298256785,46.8862095951938));
#12662=CARTESIAN_POINT('',(-19.5,1.53522655283679,46.8862095951938));
#12663=CARTESIAN_POINT('',(-19.5,-6.43177298256785,33.0141314097479));
#12664=CARTESIAN_POINT('',(-19.5,-6.43177298256785,-5.56473183187052));
#12665=CARTESIAN_POINT('',(-19.5,-6.43177298256785,26.0826265387027));
#12666=CARTESIAN_POINT('Origin',(-19.5,-5.94334688204796,29.5483789742253));
#12667=CARTESIAN_POINT('',(-19.5,-6.43177298256785,-18.9365770263474));
#12668=CARTESIAN_POINT('',(-19.5,-6.43177298256785,-5.56473183187052));
#12669=CARTESIAN_POINT('Origin',(-19.5,-6.00539963551477,-22.4105093470644));
#12670=CARTESIAN_POINT('Origin',(-0.499999999999999,25.4362251590507,30.0096109045284));
#12671=CARTESIAN_POINT('',(-0.499999999999999,25.4362251590507,-18.9365770263474));
#12672=CARTESIAN_POINT('',(-0.499999999999999,25.4362251590507,26.0826265387027));
#12673=CARTESIAN_POINT('Origin',(-0.499999999999999,-6.43177298256785,-23.0483789742253));
#12674=CARTESIAN_POINT('',(-0.499999999999999,-6.43177298256785,33.0141314097479));
#12675=CARTESIAN_POINT('',(-0.499999999999999,-6.43177298256785,46.8862095951938));
#12676=CARTESIAN_POINT('Origin',(-0.499999999999999,-6.43177298256785,-23.0483789742253));
#12677=CARTESIAN_POINT('',(-0.499999999999999,-6.43177298256785,26.0826265387027));
#12678=CARTESIAN_POINT('',(-0.499999999999999,-6.43177298256785,-18.9365770263474));
#12679=CARTESIAN_POINT('Origin',(-0.499999999999999,22.2953189477035,33.0096109045284));
#12680=CARTESIAN_POINT('',(-0.499999999999999,21.4945386978003,30.1184604429708));
#12681=CARTESIAN_POINT('',(-0.499999999999999,19.2953189477036,33.0096109045284));
#12682=CARTESIAN_POINT('Origin',(-0.499999999999999,-6.43177298256785,46.8862095951938));
#12683=CARTESIAN_POINT('',(-0.499999999999999,19.2953189477036,46.8862095951938));
#12684=CARTESIAN_POINT('Origin',(-0.499999999999999,24.9477990585308,29.5483789742253));
#12685=CARTESIAN_POINT('Origin',(-0.499999999999999,-6.00539963551477,-22.4105093470644));
#12686=CARTESIAN_POINT('Origin',(-0.499999999999999,-5.94334688204796,29.5483789742253));
#12687=CARTESIAN_POINT('Origin',(-0.499999999999999,25.0098518119976,-22.4105093470644));
#12688=CARTESIAN_POINT('Origin',(-0.499999999999999,19.2953189477036,46.8862095951938));
#12689=CARTESIAN_POINT('Origin',(-0.499999999999999,24.9477990585308,29.5483789742253));
#12690=CARTESIAN_POINT('',(-18.5,23.4477990585308,29.5483789742253));
#12691=CARTESIAN_POINT('',(-0.499999999999999,23.4477990585308,29.5483789742253));
#12692=CARTESIAN_POINT('Origin',(-18.5,24.9477990585308,29.5483789742253));
#12693=CARTESIAN_POINT('Origin',(-18.5,24.9477990585308,29.5483789742253));
#12694=CARTESIAN_POINT('Origin',(-0.499999999999999,-6.00539963551477,-22.4105093470644));
#12695=CARTESIAN_POINT('',(-18.5,-7.50539963551477,-22.4105093470644));
#12696=CARTESIAN_POINT('',(-0.499999999999999,-7.50539963551477,-22.4105093470644));
#12697=CARTESIAN_POINT('Origin',(-18.5,-6.00539963551477,-22.4105093470644));
#12698=CARTESIAN_POINT('Origin',(-18.5,-6.00539963551477,-22.4105093470644));
#12699=CARTESIAN_POINT('Origin',(-0.499999999999999,-5.94334688204796,29.5483789742253));
#12700=CARTESIAN_POINT('',(-18.5,-7.44334688204796,29.5483789742253));
#12701=CARTESIAN_POINT('',(-0.499999999999999,-7.44334688204796,29.5483789742253));
#12702=CARTESIAN_POINT('Origin',(-18.5,-5.94334688204796,29.5483789742253));
#12703=CARTESIAN_POINT('Origin',(-18.5,-5.94334688204796,29.5483789742253));
#12704=CARTESIAN_POINT('Origin',(-0.499999999999999,25.0098518119976,-22.4105093470644));
#12705=CARTESIAN_POINT('',(-18.5,23.5098518119976,-22.4105093470644));
#12706=CARTESIAN_POINT('',(-0.499999999999999,23.5098518119976,-22.4105093470644));
#12707=CARTESIAN_POINT('Origin',(-18.5,25.0098518119976,-22.4105093470644));
#12708=CARTESIAN_POINT('Origin',(-18.5,25.0098518119976,-22.4105093470644));
#12709=CARTESIAN_POINT('Origin',(-20.5,20.2953189477035,29.402562452839));
#12710=CARTESIAN_POINT('',(-21.5,20.2953189477036,46.8862095951938));
#12711=CARTESIAN_POINT('',(-20.5,21.2953189477036,46.8862095951938));
#12712=CARTESIAN_POINT('Origin',(-20.5,20.2953189477036,46.8862095951938));
#12713=CARTESIAN_POINT('',(-20.5,21.2953189477036,33.0096109045284));
#12714=CARTESIAN_POINT('',(-20.5,21.2953189477035,29.402562452839));
#12715=CARTESIAN_POINT('',(-21.5,20.2953189477035,33.0096109045284));
#12716=CARTESIAN_POINT('Origin',(-20.5,20.2953189477035,33.0096109045284));
#12717=CARTESIAN_POINT('',(-21.5,20.2953189477035,29.402562452839));
#12718=CARTESIAN_POINT('Origin',(-20.5,22.2953189477035,33.0096109045284));
#12719=CARTESIAN_POINT('',(-20.5,22.2953189477036,32.0096109045284));
#12720=CARTESIAN_POINT('',(-21.5,22.2953189477036,31.0096109045284));
#12721=CARTESIAN_POINT('Origin',(-20.5,22.2953189477036,31.0096109045284));
#12722=CARTESIAN_POINT('Origin',(-21.5,22.2953189477035,33.0096109045284));
#12723=CARTESIAN_POINT('Origin',(-20.5,22.2953189477035,33.0096109045284));
#12724=CARTESIAN_POINT('Origin',(-20.5,15.8987725179725,31.0096109045284));
#12725=CARTESIAN_POINT('',(-20.5,25.4362251590507,32.0096109045284));
#12726=CARTESIAN_POINT('',(-21.5,25.4362251590507,31.0096109045284));
#12727=CARTESIAN_POINT('Origin',(-20.5,25.4362251590507,31.0096109045284));
#12728=CARTESIAN_POINT('',(-21.5,15.8987725179725,31.0096109045284));
#12729=CARTESIAN_POINT('',(-20.5,15.8987725179725,32.0096109045284));
#12730=CARTESIAN_POINT('Ctrl Pts',(-20.5,25.4362251590507,32.0096109045284));
#12731=CARTESIAN_POINT('Ctrl Pts',(-20.5,27.4362251590507,32.0096109045285));
#12732=CARTESIAN_POINT('Ctrl Pts',(-20.5,27.4362251590507,30.0096109045284));
#12733=CARTESIAN_POINT('Ctrl Pts',(-21.5,25.4362251590507,32.0096109045284));
#12734=CARTESIAN_POINT('Ctrl Pts',(-21.5,27.4362251590507,32.0096109045285));
#12735=CARTESIAN_POINT('Ctrl Pts',(-21.5,27.4362251590507,30.0096109045284));
#12736=CARTESIAN_POINT('Ctrl Pts',(-21.5,25.4362251590507,31.0096109045284));
#12737=CARTESIAN_POINT('Ctrl Pts',(-21.5,26.4362251590507,31.0096109045284));
#12738=CARTESIAN_POINT('Ctrl Pts',(-21.5,26.4362251590507,30.0096109045284));
#12739=CARTESIAN_POINT('',(-20.5,27.4362251590507,30.0096109045284));
#12740=CARTESIAN_POINT('',(-21.5,26.4362251590507,30.0096109045284));
#12741=CARTESIAN_POINT('Origin',(-20.5,26.4362251590507,30.0096109045284));
#12742=CARTESIAN_POINT('Origin',(-21.5,25.4362251590507,30.0096109045284));
#12743=CARTESIAN_POINT('Origin',(-20.5,25.4362251590507,30.0096109045284));
#12744=CARTESIAN_POINT('Origin',(-20.5,26.4362251590507,20.9642631075063));
#12745=CARTESIAN_POINT('',(-20.5,27.4362251590507,-23.0483789742253));
#12746=CARTESIAN_POINT('',(-21.5,26.4362251590507,-23.0483789742253));
#12747=CARTESIAN_POINT('Origin',(-20.5,26.4362251590507,-23.0483789742253));
#12748=CARTESIAN_POINT('',(-21.5,26.4362251590507,20.9642631075063));
#12749=CARTESIAN_POINT('',(-20.5,27.4362251590507,20.9642631075063));
#12750=CARTESIAN_POINT('Ctrl Pts',(-20.5,27.4362251590507,-23.0483789742253));
#12751=CARTESIAN_POINT('Ctrl Pts',(-20.5,27.4362251590507,-25.0483789742253));
#12752=CARTESIAN_POINT('Ctrl Pts',(-20.5,25.4362251590507,-25.0483789742253));
#12753=CARTESIAN_POINT('Ctrl Pts',(-21.5,27.4362251590507,-23.0483789742253));
#12754=CARTESIAN_POINT('Ctrl Pts',(-21.5,27.4362251590507,-25.0483789742253));
#12755=CARTESIAN_POINT('Ctrl Pts',(-21.5,25.4362251590507,-25.0483789742253));
#12756=CARTESIAN_POINT('Ctrl Pts',(-21.5,26.4362251590507,-23.0483789742253));
#12757=CARTESIAN_POINT('Ctrl Pts',(-21.5,26.4362251590507,-24.0483789742253));
#12758=CARTESIAN_POINT('Ctrl Pts',(-21.5,25.4362251590507,-24.0483789742253));
#12759=CARTESIAN_POINT('',(-21.5,25.4362251590507,-24.0483789742253));
#12760=CARTESIAN_POINT('Origin',(-20.5,25.4362251590507,-24.0483789742253));
#12761=CARTESIAN_POINT('Origin',(-21.5,25.4362251590507,-23.0483789742253));
#12762=CARTESIAN_POINT('Origin',(-20.5,25.4362251590507,-23.0483789742253));
#12763=CARTESIAN_POINT('Origin',(-20.5,17.4692256236461,-24.0483789742253));
#12764=CARTESIAN_POINT('',(-21.5,-6.43177298256785,-24.0483789742253));
#12765=CARTESIAN_POINT('Origin',(-20.5,-6.43177298256785,-24.0483789742253));
#12766=CARTESIAN_POINT('',(-21.5,17.4692256236461,-24.0483789742253));
#12767=CARTESIAN_POINT('Ctrl Pts',(-20.5,-6.43177298256785,-25.0483789742253));
#12768=CARTESIAN_POINT('Ctrl Pts',(-20.5,-8.43177298256785,-25.0483789742253));
#12769=CARTESIAN_POINT('Ctrl Pts',(-20.5,-8.43177298256785,-23.0483789742253));
#12770=CARTESIAN_POINT('Ctrl Pts',(-21.5,-6.43177298256785,-25.0483789742253));
#12771=CARTESIAN_POINT('Ctrl Pts',(-21.5,-8.43177298256785,-25.0483789742253));
#12772=CARTESIAN_POINT('Ctrl Pts',(-21.5,-8.43177298256785,-23.0483789742253));
#12773=CARTESIAN_POINT('Ctrl Pts',(-21.5,-6.43177298256785,-24.0483789742253));
#12774=CARTESIAN_POINT('Ctrl Pts',(-21.5,-7.43177298256785,-24.0483789742253));
#12775=CARTESIAN_POINT('Ctrl Pts',(-21.5,-7.43177298256785,-23.0483789742253));
#12776=CARTESIAN_POINT('',(-20.5,-8.43177298256785,-23.0483789742253));
#12777=CARTESIAN_POINT('',(-21.5,-7.43177298256785,-23.0483789742253));
#12778=CARTESIAN_POINT('Origin',(-20.5,-7.43177298256785,-23.0483789742253));
#12779=CARTESIAN_POINT('Origin',(-21.5,-6.43177298256785,-23.0483789742253));
#12780=CARTESIAN_POINT('Origin',(-20.5,-6.43177298256785,-23.0483789742253));
#12781=CARTESIAN_POINT('Origin',(-20.5,-7.43177298256785,-5.56473183187052));
#12782=CARTESIAN_POINT('',(-20.5,-8.43177298256785,46.8862095951938));
#12783=CARTESIAN_POINT('',(-21.5,-7.43177298256786,46.8862095951938));
#12784=CARTESIAN_POINT('Origin',(-20.5,-7.43177298256786,46.8862095951938));
#12785=CARTESIAN_POINT('',(-21.5,-7.43177298256785,-5.56473183187052));
#12786=CARTESIAN_POINT('',(-20.5,-8.43177298256785,-5.56473183187052));
#12787=CARTESIAN_POINT('Ctrl Pts',(-20.5,-8.43177298256785,46.8862095951938));
#12788=CARTESIAN_POINT('Ctrl Pts',(-20.5,-8.43177298256785,48.8862095951938));
#12789=CARTESIAN_POINT('Ctrl Pts',(-20.5,-6.43177298256785,48.8862095951938));
#12790=CARTESIAN_POINT('Ctrl Pts',(-21.5,-8.43177298256785,46.8862095951938));
#12791=CARTESIAN_POINT('Ctrl Pts',(-21.5,-8.43177298256785,48.8862095951938));
#12792=CARTESIAN_POINT('Ctrl Pts',(-21.5,-6.43177298256785,48.8862095951938));
#12793=CARTESIAN_POINT('Ctrl Pts',(-21.5,-7.43177298256786,46.8862095951938));
#12794=CARTESIAN_POINT('Ctrl Pts',(-21.5,-7.43177298256785,47.8862095951938));
#12795=CARTESIAN_POINT('Ctrl Pts',(-21.5,-6.43177298256785,47.8862095951938));
#12796=CARTESIAN_POINT('',(-21.5,-6.43177298256785,47.8862095951938));
#12797=CARTESIAN_POINT('Origin',(-20.5,-6.43177298256785,47.8862095951938));
#12798=CARTESIAN_POINT('Origin',(-21.5,-6.43177298256785,46.8862095951938));
#12799=CARTESIAN_POINT('Origin',(-20.5,-6.43177298256785,46.8862095951938));
#12800=CARTESIAN_POINT('Origin',(-20.5,1.53522655283679,47.8862095951938));
#12801=CARTESIAN_POINT('',(-21.5,19.2953189477036,47.8862095951938));
#12802=CARTESIAN_POINT('Origin',(-20.5,19.2953189477036,47.8862095951938));
#12803=CARTESIAN_POINT('',(-21.5,1.53522655283679,47.8862095951938));
#12804=CARTESIAN_POINT('Ctrl Pts',(-20.5,19.2953189477036,48.8862095951938));
#12805=CARTESIAN_POINT('Ctrl Pts',(-20.5,21.2953189477036,48.8862095951938));
#12806=CARTESIAN_POINT('Ctrl Pts',(-20.5,21.2953189477036,46.8862095951938));
#12807=CARTESIAN_POINT('Ctrl Pts',(-21.5,19.2953189477036,48.8862095951938));
#12808=CARTESIAN_POINT('Ctrl Pts',(-21.5,21.2953189477036,48.8862095951938));
#12809=CARTESIAN_POINT('Ctrl Pts',(-21.5,21.2953189477036,46.8862095951938));
#12810=CARTESIAN_POINT('Ctrl Pts',(-21.5,19.2953189477036,47.8862095951938));
#12811=CARTESIAN_POINT('Ctrl Pts',(-21.5,20.2953189477036,47.8862095951938));
#12812=CARTESIAN_POINT('Ctrl Pts',(-21.5,20.2953189477036,46.8862095951938));
#12813=CARTESIAN_POINT('Origin',(-21.5,19.2953189477036,46.8862095951938));
#12814=CARTESIAN_POINT('Origin',(-20.5,19.2953189477036,46.8862095951938));
#12815=CARTESIAN_POINT('Origin',(-0.499999999999999,25.4362251590507,-23.0483789742253));
#12816=CARTESIAN_POINT('',(-0.499999999999999,27.4362251590507,-23.0483789742253));
#12817=CARTESIAN_POINT('Origin',(-0.499999999999999,27.4362251590507,30.0096109045284));
#12818=CARTESIAN_POINT('',(-0.499999999999999,27.4362251590507,30.0096109045284));
#12819=CARTESIAN_POINT('Origin',(-0.499999999999999,25.4362251590507,30.0096109045284));
#12820=CARTESIAN_POINT('',(-0.499999999999999,25.4362251590507,32.0096109045284));
#12821=CARTESIAN_POINT('Origin',(-0.499999999999999,22.2953189477036,32.0096109045284));
#12822=CARTESIAN_POINT('',(-0.499999999999999,22.2953189477036,32.0096109045284));
#12823=CARTESIAN_POINT('Origin',(-0.499999999999999,22.2953189477035,33.0096109045284));
#12824=CARTESIAN_POINT('',(-0.499999999999999,21.2953189477036,33.0096109045284));
#12825=CARTESIAN_POINT('Origin',(-0.499999999999999,21.2953189477036,46.8862095951938));
#12826=CARTESIAN_POINT('',(-0.499999999999999,21.2953189477036,46.8862095951938));
#12827=CARTESIAN_POINT('Origin',(-21.5,9.50222608824143,11.9189153104842));
#12828=CARTESIAN_POINT('Origin',(-0.499999999999999,19.2953189477036,46.8862095951938));
#12829=CARTESIAN_POINT('Origin',(-0.499999999999999,-6.43177298256785,46.8862095951938));
#12830=CARTESIAN_POINT('',(-0.499999999999999,-8.43177298256785,46.8862095951938));
#12831=CARTESIAN_POINT('Origin',(-0.499999999999999,-8.43177298256785,-23.0483789742253));
#12832=CARTESIAN_POINT('',(-0.499999999999999,-8.43177298256785,-23.0483789742253));
#12833=CARTESIAN_POINT('Origin',(-0.499999999999999,-6.43177298256785,-23.0483789742253));
#12834=CARTESIAN_POINT('',(0.,0.,0.));
#12835=CARTESIAN_POINT('Origin',(-6.5,6.43177298256785,249.937669285906));
#12836=CARTESIAN_POINT('',(4.5,3.23177298256785,249.937669285906));
#12837=CARTESIAN_POINT('Origin',(4.5,6.43177298256785,249.937669285906));
#12838=CARTESIAN_POINT('',(5.5,3.23177298256785,249.937669285906));
#12839=CARTESIAN_POINT('',(-6.5,3.23177298256785,249.937669285906));
#12840=CARTESIAN_POINT('Origin',(5.5,6.43177298256785,249.937669285906));
#12841=CARTESIAN_POINT('Origin',(-6.5,6.43177298256785,249.937669285906));
#12842=CARTESIAN_POINT('',(-18.5,3.23177298256785,249.937669285906));
#12843=CARTESIAN_POINT('Origin',(-18.5,6.43177298256785,249.937669285906));
#12844=CARTESIAN_POINT('',(-17.5,3.23177298256785,249.937669285906));
#12845=CARTESIAN_POINT('',(-6.5,3.23177298256785,249.937669285906));
#12846=CARTESIAN_POINT('Origin',(-17.5,6.43177298256785,249.937669285906));
#12847=CARTESIAN_POINT('Origin',(-6.5,6.43177298256785,44.0628614786648));
#12848=CARTESIAN_POINT('',(4.5,3.23177298256785,44.0628614786648));
#12849=CARTESIAN_POINT('Origin',(4.5,6.43177298256785,44.0628614786648));
#12850=CARTESIAN_POINT('',(5.5,3.23177298256785,44.0628614786648));
#12851=CARTESIAN_POINT('',(-6.5,3.23177298256785,44.0628614786648));
#12852=CARTESIAN_POINT('Origin',(5.5,6.43177298256785,44.0628614786648));
#12853=CARTESIAN_POINT('Origin',(-6.5,6.43177298256785,44.0628614786648));
#12854=CARTESIAN_POINT('',(-18.5,3.23177298256785,44.0628614786648));
#12855=CARTESIAN_POINT('Origin',(-18.5,6.43177298256785,44.0628614786648));
#12856=CARTESIAN_POINT('',(-17.5,3.23177298256785,44.0628614786648));
#12857=CARTESIAN_POINT('',(-6.5,3.23177298256785,44.0628614786648));
#12858=CARTESIAN_POINT('Origin',(-17.5,6.43177298256785,44.0628614786648));
#12859=CARTESIAN_POINT('Origin',(-6.5,6.43177298256785,36.8862095951938));
#12860=CARTESIAN_POINT('',(-18.5,16.4317729825678,36.8862095951938));
#12861=CARTESIAN_POINT('',(-16.5,18.4317729825679,36.8862095951938));
#12862=CARTESIAN_POINT('Origin',(-16.5,16.4317729825679,36.8862095951938));
#12863=CARTESIAN_POINT('',(3.5,18.4317729825679,36.8862095951938));
#12864=CARTESIAN_POINT('',(-0.499999999999999,18.4317729825679,36.8862095951938));
#12865=CARTESIAN_POINT('',(5.5,16.4317729825678,36.8862095951938));
#12866=CARTESIAN_POINT('Origin',(3.5,16.4317729825679,36.8862095951938));
#12867=CARTESIAN_POINT('',(5.5,-3.56822701743215,36.8862095951938));
#12868=CARTESIAN_POINT('',(5.5,16.4317729825678,36.8862095951938));
#12869=CARTESIAN_POINT('',(3.5,-5.56822701743215,36.8862095951938));
#12870=CARTESIAN_POINT('Origin',(3.5,-3.56822701743215,36.8862095951938));
#12871=CARTESIAN_POINT('',(-16.5,-5.56822701743215,36.8862095951938));
#12872=CARTESIAN_POINT('',(-0.499999999999999,-5.56822701743215,36.8862095951938));
#12873=CARTESIAN_POINT('',(-18.5,-3.56822701743215,36.8862095951938));
#12874=CARTESIAN_POINT('Origin',(-16.5,-3.56822701743215,36.8862095951938));
#12875=CARTESIAN_POINT('',(-18.5,-3.56822701743215,36.8862095951938));
#12876=CARTESIAN_POINT('',(4.5,16.4317729825679,36.8862095951938));
#12877=CARTESIAN_POINT('',(3.5,17.4317729825679,36.8862095951938));
#12878=CARTESIAN_POINT('Origin',(3.5,16.4317729825679,36.8862095951938));
#12879=CARTESIAN_POINT('',(-16.5,17.4317729825679,36.8862095951938));
#12880=CARTESIAN_POINT('',(-0.499999999999999,17.4317729825679,36.8862095951938));
#12881=CARTESIAN_POINT('',(-17.5,16.4317729825678,36.8862095951938));
#12882=CARTESIAN_POINT('Origin',(-16.5,16.4317729825679,36.8862095951938));
#12883=CARTESIAN_POINT('',(-17.5,-3.56822701743215,36.8862095951938));
#12884=CARTESIAN_POINT('',(-17.5,-3.56822701743215,36.8862095951938));
#12885=CARTESIAN_POINT('',(-16.5,-4.56822701743215,36.8862095951938));
#12886=CARTESIAN_POINT('Origin',(-16.5,-3.56822701743215,36.8862095951938));
#12887=CARTESIAN_POINT('',(3.5,-4.56822701743215,36.8862095951938));
#12888=CARTESIAN_POINT('',(-0.499999999999999,-4.56822701743215,36.8862095951938));
#12889=CARTESIAN_POINT('',(4.5,-3.56822701743214,36.8862095951938));
#12890=CARTESIAN_POINT('Origin',(3.5,-3.56822701743215,36.8862095951938));
#12891=CARTESIAN_POINT('',(4.5,16.4317729825679,36.8862095951938));
#12892=CARTESIAN_POINT('Origin',(-16.5,17.4317729825679,48.8862095951938));
#12893=CARTESIAN_POINT('',(3.5,17.4317729825679,256.886209595194));
#12894=CARTESIAN_POINT('',(3.5,17.4317729825679,48.8862095951938));
#12895=CARTESIAN_POINT('',(-16.5,17.4317729825679,256.886209595194));
#12896=CARTESIAN_POINT('',(-0.499999999999999,17.4317729825679,256.886209595194));
#12897=CARTESIAN_POINT('',(-16.5,17.4317729825679,48.8862095951938));
#12898=CARTESIAN_POINT('Origin',(-16.5,16.4317729825679,48.8862095951938));
#12899=CARTESIAN_POINT('',(-17.5,16.4317729825678,256.886209595194));
#12900=CARTESIAN_POINT('Origin',(-16.5,16.4317729825679,256.886209595194));
#12901=CARTESIAN_POINT('',(-17.5,16.4317729825678,48.8862095951938));
#12902=CARTESIAN_POINT('Origin',(-17.5,-3.56822701743215,48.8862095951938));
#12903=CARTESIAN_POINT('',(-17.5,-3.56822701743215,256.886209595194));
#12904=CARTESIAN_POINT('',(-17.5,-3.56822701743215,256.886209595194));
#12905=CARTESIAN_POINT('',(-17.5,-3.56822701743215,48.8862095951938));
#12906=CARTESIAN_POINT('Origin',(-16.5,-3.56822701743215,48.8862095951938));
#12907=CARTESIAN_POINT('',(-16.5,-4.56822701743215,256.886209595194));
#12908=CARTESIAN_POINT('Origin',(-16.5,-3.56822701743215,256.886209595194));
#12909=CARTESIAN_POINT('',(-16.5,-4.56822701743215,48.8862095951938));
#12910=CARTESIAN_POINT('Origin',(3.5,-4.56822701743215,48.8862095951938));
#12911=CARTESIAN_POINT('',(3.5,-4.56822701743215,256.886209595194));
#12912=CARTESIAN_POINT('',(-0.499999999999999,-4.56822701743215,256.886209595194));
#12913=CARTESIAN_POINT('',(3.5,-4.56822701743215,48.8862095951938));
#12914=CARTESIAN_POINT('Origin',(3.5,-3.56822701743215,48.8862095951938));
#12915=CARTESIAN_POINT('',(4.5,-3.56822701743214,256.886209595194));
#12916=CARTESIAN_POINT('Origin',(3.5,-3.56822701743215,256.886209595194));
#12917=CARTESIAN_POINT('',(4.5,-3.56822701743215,48.8862095951938));
#12918=CARTESIAN_POINT('Origin',(4.5,16.4317729825679,48.8862095951938));
#12919=CARTESIAN_POINT('',(4.5,16.4317729825679,256.886209595194));
#12920=CARTESIAN_POINT('',(4.5,16.4317729825679,256.886209595194));
#12921=CARTESIAN_POINT('',(4.5,16.4317729825679,48.8862095951938));
#12922=CARTESIAN_POINT('Origin',(3.5,16.4317729825679,48.8862095951938));
#12923=CARTESIAN_POINT('Origin',(3.5,16.4317729825679,256.886209595194));
#12924=CARTESIAN_POINT('Origin',(3.5,18.4317729825679,48.8862095951938));
#12925=CARTESIAN_POINT('',(-16.5,18.4317729825679,256.886209595194));
#12926=CARTESIAN_POINT('',(-16.5,18.4317729825679,48.8862095951938));
#12927=CARTESIAN_POINT('',(3.5,18.4317729825679,256.886209595194));
#12928=CARTESIAN_POINT('',(-0.499999999999999,18.4317729825679,256.886209595194));
#12929=CARTESIAN_POINT('',(3.5,18.4317729825679,48.8862095951938));
#12930=CARTESIAN_POINT('Origin',(3.5,16.4317729825679,48.8862095951938));
#12931=CARTESIAN_POINT('',(5.5,16.4317729825678,256.886209595194));
#12932=CARTESIAN_POINT('Origin',(3.5,16.4317729825679,256.886209595194));
#12933=CARTESIAN_POINT('',(5.5,16.4317729825678,48.8862095951938));
#12934=CARTESIAN_POINT('Origin',(5.5,-3.56822701743215,48.8862095951938));
#12935=CARTESIAN_POINT('',(5.5,-3.56822701743215,256.886209595194));
#12936=CARTESIAN_POINT('',(5.5,16.4317729825678,256.886209595194));
#12937=CARTESIAN_POINT('',(5.5,-3.56822701743215,48.8862095951938));
#12938=CARTESIAN_POINT('Origin',(3.5,-3.56822701743215,48.8862095951938));
#12939=CARTESIAN_POINT('',(3.5,-5.56822701743215,256.886209595194));
#12940=CARTESIAN_POINT('Origin',(3.5,-3.56822701743215,256.886209595194));
#12941=CARTESIAN_POINT('',(3.5,-5.56822701743215,48.8862095951938));
#12942=CARTESIAN_POINT('Origin',(-16.5,-5.56822701743215,48.8862095951938));
#12943=CARTESIAN_POINT('',(-16.5,-5.56822701743215,256.886209595194));
#12944=CARTESIAN_POINT('',(-0.499999999999999,-5.56822701743215,256.886209595194));
#12945=CARTESIAN_POINT('',(-16.5,-5.56822701743215,48.8862095951938));
#12946=CARTESIAN_POINT('Origin',(-16.5,-3.56822701743215,48.8862095951938));
#12947=CARTESIAN_POINT('',(-18.5,-3.56822701743215,256.886209595194));
#12948=CARTESIAN_POINT('Origin',(-16.5,-3.56822701743215,256.886209595194));
#12949=CARTESIAN_POINT('',(-18.5,-3.56822701743215,48.8862095951938));
#12950=CARTESIAN_POINT('Origin',(-18.5,16.4317729825678,48.8862095951938));
#12951=CARTESIAN_POINT('',(-18.5,16.4317729825678,256.886209595194));
#12952=CARTESIAN_POINT('',(-18.5,-3.56822701743215,256.886209595194));
#12953=CARTESIAN_POINT('',(-18.5,16.4317729825678,48.8862095951938));
#12954=CARTESIAN_POINT('Origin',(-16.5,16.4317729825679,48.8862095951938));
#12955=CARTESIAN_POINT('Origin',(-16.5,16.4317729825679,256.886209595194));
#12956=CARTESIAN_POINT('Origin',(-6.5,6.43177298256785,256.886209595194));
#12957=CARTESIAN_POINT('',(0.,0.,0.));
#12958=CARTESIAN_POINT('Origin',(3.5,1.43177298256785,258.886209595194));
#12959=CARTESIAN_POINT('',(3.5,-3.56822701743216,260.886209595194));
#12960=CARTESIAN_POINT('',(5.5,-3.56822701743215,258.886209595194));
#12961=CARTESIAN_POINT('Origin',(3.5,-3.56822701743215,258.886209595194));
#12962=CARTESIAN_POINT('',(5.5,16.4317729825678,258.886209595194));
#12963=CARTESIAN_POINT('',(5.5,1.43177298256785,258.886209595194));
#12964=CARTESIAN_POINT('',(3.5,16.4317729825678,260.886209595194));
#12965=CARTESIAN_POINT('Origin',(3.5,16.4317729825678,258.886209595194));
#12966=CARTESIAN_POINT('',(3.5,1.43177298256785,260.886209595194));
#12967=CARTESIAN_POINT('Origin',(-1.5,16.4317729825679,258.886209595194));
#12968=CARTESIAN_POINT('',(3.5,18.4317729825679,258.886209595194));
#12969=CARTESIAN_POINT('Origin',(3.5,16.4317729825679,258.886209595194));
#12970=CARTESIAN_POINT('',(-16.5,18.4317729825679,258.886209595194));
#12971=CARTESIAN_POINT('',(-1.5,18.4317729825679,258.886209595194));
#12972=CARTESIAN_POINT('',(-16.5,16.4317729825679,260.886209595194));
#12973=CARTESIAN_POINT('Origin',(-16.5,16.4317729825679,258.886209595194));
#12974=CARTESIAN_POINT('',(-1.5,16.4317729825679,260.886209595194));
#12975=CARTESIAN_POINT('Origin',(3.5,16.4317729825678,258.886209595194));
#12976=CARTESIAN_POINT('Origin',(3.5,16.4317729825678,258.886209595194));
#12977=CARTESIAN_POINT('Origin',(-16.5,11.4317729825679,258.886209595194));
#12978=CARTESIAN_POINT('',(-18.5,16.4317729825679,258.886209595194));
#12979=CARTESIAN_POINT('Origin',(-16.5,16.4317729825679,258.886209595194));
#12980=CARTESIAN_POINT('',(-18.5,-3.56822701743215,258.886209595194));
#12981=CARTESIAN_POINT('',(-18.5,11.4317729825679,258.886209595194));
#12982=CARTESIAN_POINT('',(-16.5,-3.56822701743215,260.886209595194));
#12983=CARTESIAN_POINT('Origin',(-16.5,-3.56822701743215,258.886209595194));
#12984=CARTESIAN_POINT('',(-16.5,11.4317729825679,260.886209595194));
#12985=CARTESIAN_POINT('Origin',(-16.5,16.4317729825679,258.886209595194));
#12986=CARTESIAN_POINT('Origin',(-16.5,16.4317729825679,258.886209595194));
#12987=CARTESIAN_POINT('Origin',(-11.5,-3.56822701743215,258.886209595194));
#12988=CARTESIAN_POINT('',(-16.5,-5.56822701743215,258.886209595194));
#12989=CARTESIAN_POINT('Origin',(-16.5,-3.56822701743215,258.886209595194));
#12990=CARTESIAN_POINT('',(3.5,-5.56822701743215,258.886209595194));
#12991=CARTESIAN_POINT('',(-11.5,-5.56822701743215,258.886209595194));
#12992=CARTESIAN_POINT('Origin',(3.5,-3.56822701743216,258.886209595194));
#12993=CARTESIAN_POINT('',(-11.5,-3.56822701743215,260.886209595194));
#12994=CARTESIAN_POINT('Origin',(-16.5,-3.56822701743215,258.886209595194));
#12995=CARTESIAN_POINT('Origin',(-16.5,-3.56822701743215,258.886209595194));
#12996=CARTESIAN_POINT('Origin',(3.5,-3.56822701743215,258.886209595194));
#12997=CARTESIAN_POINT('Origin',(3.5,-3.56822701743215,258.886209595194));
#12998=CARTESIAN_POINT('Origin',(3.5,16.4317729825678,256.886209595194));
#12999=CARTESIAN_POINT('',(5.5,16.4317729825678,256.886209595194));
#13000=CARTESIAN_POINT('',(5.5,16.4317729825678,256.886209595194));
#13001=CARTESIAN_POINT('',(3.5,18.4317729825679,256.886209595194));
#13002=CARTESIAN_POINT('Origin',(3.5,16.4317729825678,256.886209595194));
#13003=CARTESIAN_POINT('',(3.5,18.4317729825679,256.886209595194));
#13004=CARTESIAN_POINT('Origin',(5.5,-3.56822701743215,256.886209595194));
#13005=CARTESIAN_POINT('',(5.5,-3.56822701743215,256.886209595194));
#13006=CARTESIAN_POINT('',(5.5,-3.56822701743215,256.886209595194));
#13007=CARTESIAN_POINT('',(5.5,-3.56822701743215,256.886209595194));
#13008=CARTESIAN_POINT('Origin',(3.5,-3.56822701743215,256.886209595194));
#13009=CARTESIAN_POINT('',(3.5,-5.56822701743215,256.886209595194));
#13010=CARTESIAN_POINT('',(3.5,-5.56822701743215,256.886209595194));
#13011=CARTESIAN_POINT('Origin',(3.5,-3.56822701743215,256.886209595194));
#13012=CARTESIAN_POINT('Origin',(-16.5,-5.56822701743215,256.886209595194));
#13013=CARTESIAN_POINT('',(-16.5,-5.56822701743215,256.886209595194));
#13014=CARTESIAN_POINT('',(-16.5,-5.56822701743215,256.886209595194));
#13015=CARTESIAN_POINT('',(-16.5,-5.56822701743215,256.886209595194));
#13016=CARTESIAN_POINT('Origin',(-6.5,6.43177298256785,260.886209595194));
#13017=CARTESIAN_POINT('',(-15.5,6.43177298256785,260.886209595194));
#13018=CARTESIAN_POINT('Origin',(-6.5,6.43177298256785,260.886209595194));
#13019=CARTESIAN_POINT('Origin',(-10.6406655616155,14.6473002758614,247.086209595194));
#13020=CARTESIAN_POINT('',(-10.6406655616155,14.8473002758614,247.086209595194));
#13021=CARTESIAN_POINT('',(-10.5506510928848,14.468701856442,247.086209595194));
#13022=CARTESIAN_POINT('Origin',(-10.6406655616155,14.6473002758614,247.086209595194));
#13023=CARTESIAN_POINT('',(-10.6406655616155,14.6473002758614,246.886209595194));
#13024=CARTESIAN_POINT('Origin',(-10.6406655616155,14.6473002758614,247.086209595194));
#13025=CARTESIAN_POINT('Origin',(-10.6406655616155,14.6473002758614,247.086209595194));
#13026=CARTESIAN_POINT('Origin',(-10.6406655616156,14.6473002758614,256.886209595194));
#13027=CARTESIAN_POINT('',(-10.6406655616156,14.8473002758614,250.657383286513));
#13028=CARTESIAN_POINT('',(-10.5506510928848,14.468701856442,250.657383286513));
#13029=CARTESIAN_POINT('Origin',(-10.6406655616156,14.6473002758614,250.657383286513));
#13030=CARTESIAN_POINT('',(-10.5506510928848,14.468701856442,256.886209595194));
#13031=CARTESIAN_POINT('',(-10.6406655616156,14.8473002758614,256.886209595194));
#13032=CARTESIAN_POINT('Ctrl Pts',(-10.6406655616155,14.8473002758614,250.657383286513));
#13033=CARTESIAN_POINT('Ctrl Pts',(-10.6406655616155,14.8473002758614,250.772822299168));
#13034=CARTESIAN_POINT('Ctrl Pts',(-10.538120734944,14.8908595770985,250.995273591613));
#13035=CARTESIAN_POINT('Ctrl Pts',(-10.3384894997035,14.9691998711056,251.141377231877));
#13036=CARTESIAN_POINT('Ctrl Pts',(-10.2310529316636,15.0089220887177,251.202472284128));
#13037=CARTESIAN_POINT('Ctrl Pts',(-10.5897180129765,14.8473002758614,250.657383286513));
#13038=CARTESIAN_POINT('Ctrl Pts',(-10.5897180129765,14.8473002758614,250.761141960988));
#13039=CARTESIAN_POINT('Ctrl Pts',(-10.4974067252999,14.881909580796,250.965068827275));
#13040=CARTESIAN_POINT('Ctrl Pts',(-10.305922542976,14.9524957418658,251.110832462786));
#13041=CARTESIAN_POINT('Ctrl Pts',(-10.2016668934649,14.9892426247285,251.172204138164));
#13042=CARTESIAN_POINT('Ctrl Pts',(-10.4881554517255,14.8062503675603,250.657383286512));
#13043=CARTESIAN_POINT('Ctrl Pts',(-10.4881554517255,14.8062503675603,250.742595721283));
#13044=CARTESIAN_POINT('Ctrl Pts',(-10.4162137192475,14.8272257027818,250.918324937551));
#13045=CARTESIAN_POINT('Ctrl Pts',(-10.2409200923139,14.8880763812795,251.067105998786));
#13046=CARTESIAN_POINT('Ctrl Pts',(-10.1430306190524,14.921491757668,251.130326463532));
#13047=CARTESIAN_POINT('Ctrl Pts',(-10.4201854941467,14.6565138525604,250.657383286513));
#13048=CARTESIAN_POINT('Ctrl Pts',(-10.4201854941467,14.6565138525604,250.744356284269));
#13049=CARTESIAN_POINT('Ctrl Pts',(-10.3574107201025,14.6791700163663,250.925879494604));
#13050=CARTESIAN_POINT('Ctrl Pts',(-10.190502594735,14.7458320313741,251.084602237115));
#13051=CARTESIAN_POINT('Ctrl Pts',(-10.0960822918466,14.782338215616,251.152000580692));
#13052=CARTESIAN_POINT('Ctrl Pts',(-10.4659883159327,14.5274464330055,250.657383286513));
#13053=CARTESIAN_POINT('Ctrl Pts',(-10.4659883159327,14.5274464330055,250.769730689183));
#13054=CARTESIAN_POINT('Ctrl Pts',(-10.3869339431387,14.5654984247408,250.993661589234));
#13055=CARTESIAN_POINT('Ctrl Pts',(-10.2083950877898,14.6468617222379,251.161662391349));
#13056=CARTESIAN_POINT('Ctrl Pts',(-10.1097392710433,14.6894222004357,251.232425194565));
#13057=CARTESIAN_POINT('Ctrl Pts',(-10.5279032137342,14.4801668977517,250.657383286513));
#13058=CARTESIAN_POINT('Ctrl Pts',(-10.5279032137342,14.4801668977517,250.789388896832));
#13059=CARTESIAN_POINT('Ctrl Pts',(-10.4330225721765,14.5282019689485,251.045597317344));
#13060=CARTESIAN_POINT('Ctrl Pts',(-10.2421023786097,14.6177277546944,251.219068720891));
#13061=CARTESIAN_POINT('Ctrl Pts',(-10.138683251246,14.6634274904892,251.291741549006));
#13062=CARTESIAN_POINT('Ctrl Pts',(-10.5506510928848,14.468701856442,250.657383286513));
#13063=CARTESIAN_POINT('Ctrl Pts',(-10.5506510928848,14.468701856442,250.795910101699));
#13064=CARTESIAN_POINT('Ctrl Pts',(-10.4503355015756,14.519836688329,251.062851652633));
#13065=CARTESIAN_POINT('Ctrl Pts',(-10.2550440757969,14.6118013812939,251.23817602095));
#13066=CARTESIAN_POINT('Ctrl Pts',(-10.1499430853231,14.6584318106646,251.311490083651));
#13067=CARTESIAN_POINT('',(-10.2310529316636,15.0089220887177,251.202472284128));
#13068=CARTESIAN_POINT('',(-10.1499430853231,14.6584318106646,251.311490083651));
#13069=CARTESIAN_POINT('Origin',(-10.2310529316636,14.841246451289,251.311490083651));
#13070=CARTESIAN_POINT('Ctrl Pts',(-10.1499430853231,14.6584318106646,251.311490083651));
#13071=CARTESIAN_POINT('Ctrl Pts',(-10.2550440757969,14.6118013812939,251.23817602095));
#13072=CARTESIAN_POINT('Ctrl Pts',(-10.4503355015756,14.519836688329,251.062851652633));
#13073=CARTESIAN_POINT('Ctrl Pts',(-10.5506510928848,14.468701856442,250.795910101699));
#13074=CARTESIAN_POINT('Ctrl Pts',(-10.5506510928848,14.468701856442,250.657383286513));
#13075=CARTESIAN_POINT('Ctrl Pts',(-10.6406655616155,14.8473002758614,250.657383286513));
#13076=CARTESIAN_POINT('Ctrl Pts',(-10.6406655616155,14.8473002758614,250.772822299168));
#13077=CARTESIAN_POINT('Ctrl Pts',(-10.538120734944,14.8908595770985,250.995273591613));
#13078=CARTESIAN_POINT('Ctrl Pts',(-10.3384894997035,14.9691998711056,251.141377231877));
#13079=CARTESIAN_POINT('Ctrl Pts',(-10.2310529316636,15.0089220887177,251.202472284128));
#13080=CARTESIAN_POINT('Ctrl Pts',(-10.2310529316636,15.0089220887177,251.202472284128));
#13081=CARTESIAN_POINT('Ctrl Pts',(-9.22773159688035,15.4540682707548,251.887132680399));
#13082=CARTESIAN_POINT('Ctrl Pts',(-7.42162795596114,15.8927893964761,252.561910971013));
#13083=CARTESIAN_POINT('Ctrl Pts',(-4.84661911018312,15.73844540057,252.324521040102));
#13084=CARTESIAN_POINT('Ctrl Pts',(-3.43782795819191,15.3056862100758,251.658912548309));
#13085=CARTESIAN_POINT('Ctrl Pts',(-2.76894706833641,15.0089220887177,251.202472284128));
#13086=CARTESIAN_POINT('Ctrl Pts',(-10.2016668934649,14.9892426247285,251.172204138164));
#13087=CARTESIAN_POINT('Ctrl Pts',(-9.20327283417141,15.431382290481,251.852198827549));
#13088=CARTESIAN_POINT('Ctrl Pts',(-7.41197152048377,15.8650501229424,252.519151822071));
#13089=CARTESIAN_POINT('Ctrl Pts',(-4.8634067476038,15.7126700064094,252.284802719314));
#13090=CARTESIAN_POINT('Ctrl Pts',(-3.46392914606411,15.2840024018968,251.625533931087));
#13091=CARTESIAN_POINT('Ctrl Pts',(-2.79833310653512,14.9892426247285,251.172204138164));
#13092=CARTESIAN_POINT('Ctrl Pts',(-10.1430306190534,14.9214917576807,251.130326463525));
#13093=CARTESIAN_POINT('Ctrl Pts',(-9.15449162417327,15.3560276990127,251.802015417513));
#13094=CARTESIAN_POINT('Ctrl Pts',(-7.39262374638816,15.7776019247494,252.454602616968));
#13095=CARTESIAN_POINT('Ctrl Pts',(-4.89695559334381,15.6298815734355,252.225862811528));
#13096=CARTESIAN_POINT('Ctrl Pts',(-3.51599537753336,15.2111823852354,251.578119099517));
#13097=CARTESIAN_POINT('Ctrl Pts',(-2.85696938094662,14.9214917576808,251.130326463525));
#13098=CARTESIAN_POINT('Ctrl Pts',(-10.0960822918478,14.7823382156223,251.152000580689));
#13099=CARTESIAN_POINT('Ctrl Pts',(-9.11745075691728,15.2086150138118,251.821482469268));
#13100=CARTESIAN_POINT('Ctrl Pts',(-7.37894869396555,15.6193010674826,252.469869887398));
#13101=CARTESIAN_POINT('Ctrl Pts',(-4.92106363262171,15.4756382751295,252.242792745249));
#13102=CARTESIAN_POINT('Ctrl Pts',(-3.55633873143921,15.0665227477487,251.598321839742));
#13103=CARTESIAN_POINT('Ctrl Pts',(-2.90391770815218,14.7823382156223,251.152000580689));
#13104=CARTESIAN_POINT('Ctrl Pts',(-10.1097392710443,14.689422200441,251.232425194563));
#13105=CARTESIAN_POINT('Ctrl Pts',(-9.13234066037412,15.1172900370079,251.909075130909));
#13106=CARTESIAN_POINT('Ctrl Pts',(-7.38629562289862,15.5332576390045,252.569858388844));
#13107=CARTESIAN_POINT('Ctrl Pts',(-4.90876172522952,15.3874061283022,252.337941576935));
#13108=CARTESIAN_POINT('Ctrl Pts',(-3.54185980273583,14.9746674248189,251.683525152127));
#13109=CARTESIAN_POINT('Ctrl Pts',(-2.89026072895573,14.689422200441,251.232425194563));
#13110=CARTESIAN_POINT('Ctrl Pts',(-10.138683251246,14.6634274904892,251.291741549006));
#13111=CARTESIAN_POINT('Ctrl Pts',(-9.15845858332119,15.0967361952484,251.97440989295));
#13112=CARTESIAN_POINT('Ctrl Pts',(-7.39747124224787,15.5223048250492,252.645709370518));
#13113=CARTESIAN_POINT('Ctrl Pts',(-4.8896809061876,15.3727131232182,252.409679681977));
#13114=CARTESIAN_POINT('Ctrl Pts',(-3.51479986070389,14.9522999603287,251.746853778302));
#13115=CARTESIAN_POINT('Ctrl Pts',(-2.86131674875402,14.6634274904892,251.291741549006));
#13116=CARTESIAN_POINT('Ctrl Pts',(-10.1499430853231,14.6584318106646,251.311490083651));
#13117=CARTESIAN_POINT('Ctrl Pts',(-9.16843308390469,15.0939009017879,251.996150479922));
#13118=CARTESIAN_POINT('Ctrl Pts',(-7.40159256561416,15.5230846117326,252.670928770536));
#13119=CARTESIAN_POINT('Ctrl Pts',(-4.88256217300522,15.3720959200853,252.433538839625));
#13120=CARTESIAN_POINT('Ctrl Pts',(-3.50439691562252,14.9487445380801,251.767930347832));
#13121=CARTESIAN_POINT('Ctrl Pts',(-2.85005691467692,14.6584318106646,251.311490083651));
#13122=CARTESIAN_POINT('',(-2.76894706833642,15.0089220887177,251.202472284128));
#13123=CARTESIAN_POINT('',(-2.85005691467693,14.6584318106646,251.311490083651));
#13124=CARTESIAN_POINT('Origin',(-2.76894706833642,14.841246451289,251.311490083651));
#13125=CARTESIAN_POINT('Origin',(-6.5,6.43177298256785,238.377236865592));
#13126=CARTESIAN_POINT('Origin',(-6.5,6.59944861999658,238.268219066069));
#13127=CARTESIAN_POINT('Ctrl Pts',(-2.7689470683364,15.0089220887177,251.202472284128));
#13128=CARTESIAN_POINT('Ctrl Pts',(-2.66150284572828,14.9691970410038,251.141372879018));
#13129=CARTESIAN_POINT('Ctrl Pts',(-2.46188597582478,14.8908631544399,250.995305022995));
#13130=CARTESIAN_POINT('Ctrl Pts',(-2.35933443838445,14.8473002758614,250.772830523889));
#13131=CARTESIAN_POINT('Ctrl Pts',(-2.35933443838446,14.8473002758614,250.657383286513));
#13132=CARTESIAN_POINT('Ctrl Pts',(-2.7983331065351,14.9892426247285,251.172204138164));
#13133=CARTESIAN_POINT('Ctrl Pts',(-2.69407002908775,14.9524931237486,251.110828090218));
#13134=CARTESIAN_POINT('Ctrl Pts',(-2.50259872954677,14.8819120216761,250.965097541818));
#13135=CARTESIAN_POINT('Ctrl Pts',(-2.41028198702348,14.8473002758614,250.761149353516));
#13136=CARTESIAN_POINT('Ctrl Pts',(-2.41028198702349,14.8473002758614,250.657383286513));
#13137=CARTESIAN_POINT('Ctrl Pts',(-2.85696936415237,14.9214919773635,251.130326345305));
#13138=CARTESIAN_POINT('Ctrl Pts',(-2.75907291652762,14.8880742202187,251.067101376269));
#13139=CARTESIAN_POINT('Ctrl Pts',(-2.58378919283628,14.8272266541689,250.91834948267));
#13140=CARTESIAN_POINT('Ctrl Pts',(-2.51184450813729,14.8062507365839,250.742601792441));
#13141=CARTESIAN_POINT('Ctrl Pts',(-2.5118445081373,14.8062507365839,250.657383286513));
#13142=CARTESIAN_POINT('Ctrl Pts',(-2.90391768707942,14.7823383248995,251.152000540521));
#13143=CARTESIAN_POINT('Ctrl Pts',(-2.80949065699697,14.7458295396896,251.084597394993));
#13144=CARTESIAN_POINT('Ctrl Pts',(-2.64259110444924,14.6791708676688,250.92590490699));
#13145=CARTESIAN_POINT('Ctrl Pts',(-2.5798144560163,14.6565140249316,250.744362480863));
#13146=CARTESIAN_POINT('Ctrl Pts',(-2.57981445601631,14.6565140249316,250.657383286513));
#13147=CARTESIAN_POINT('Ctrl Pts',(-2.89026071151903,14.6894222918615,251.232425160676));
#13148=CARTESIAN_POINT('Ctrl Pts',(-2.79159786580937,14.6468587813434,251.161657315799));
#13149=CARTESIAN_POINT('Ctrl Pts',(-2.613069944193,14.5655011103562,250.993693104898));
#13150=CARTESIAN_POINT('Ctrl Pts',(-2.53401164238394,14.5274465772739,250.769738693635));
#13151=CARTESIAN_POINT('Ctrl Pts',(-2.53401164238394,14.5274465772739,250.657383286513));
#13152=CARTESIAN_POINT('Ctrl Pts',(-2.861316748754,14.6634274904892,251.291741549006));
#13153=CARTESIAN_POINT('Ctrl Pts',(-2.75789025305402,14.6177244987105,251.219063543146));
#13154=CARTESIAN_POINT('Ctrl Pts',(-2.56698332287745,14.5282057767213,251.045633492924));
#13155=CARTESIAN_POINT('Ctrl Pts',(-2.47209678626579,14.4801668977517,250.789398301879));
#13156=CARTESIAN_POINT('Ctrl Pts',(-2.4720967862658,14.4801668977517,250.657383286513));
#13157=CARTESIAN_POINT('Ctrl Pts',(-2.8500569146769,14.6584318106646,251.311490083651));
#13158=CARTESIAN_POINT('Ctrl Pts',(-2.74494843603853,14.6117980590005,251.238170797519));
#13159=CARTESIAN_POINT('Ctrl Pts',(-2.54967106330685,14.5198408878167,251.062889370291));
#13160=CARTESIAN_POINT('Ctrl Pts',(-2.44934890711523,14.468701856442,250.795919971364));
#13161=CARTESIAN_POINT('Ctrl Pts',(-2.44934890711523,14.468701856442,250.657383286513));
#13162=CARTESIAN_POINT('',(-2.35933443838446,14.8473002758614,250.657383286513));
#13163=CARTESIAN_POINT('',(-2.44934890711523,14.468701856442,250.657383286513));
#13164=CARTESIAN_POINT('Origin',(-2.35933443838446,14.6473002758614,250.657383286513));
#13165=CARTESIAN_POINT('Ctrl Pts',(-2.44934890711523,14.468701856442,250.657383286513));
#13166=CARTESIAN_POINT('Ctrl Pts',(-2.44934890711523,14.468701856442,250.795919971364));
#13167=CARTESIAN_POINT('Ctrl Pts',(-2.54967106330685,14.5198408878167,251.062889370291));
#13168=CARTESIAN_POINT('Ctrl Pts',(-2.74494843603853,14.6117980590005,251.238170797519));
#13169=CARTESIAN_POINT('Ctrl Pts',(-2.8500569146769,14.6584318106646,251.311490083651));
#13170=CARTESIAN_POINT('Ctrl Pts',(-2.7689470683364,15.0089220887177,251.202472284128));
#13171=CARTESIAN_POINT('Ctrl Pts',(-2.66150284572828,14.9691970410038,251.141372879018));
#13172=CARTESIAN_POINT('Ctrl Pts',(-2.46188597582478,14.8908631544399,250.995305022995));
#13173=CARTESIAN_POINT('Ctrl Pts',(-2.35933443838445,14.8473002758614,250.772830523889));
#13174=CARTESIAN_POINT('Ctrl Pts',(-2.35933443838446,14.8473002758614,250.657383286513));
#13175=CARTESIAN_POINT('Origin',(-2.35933443838445,14.6473002758614,256.886209595194));
#13176=CARTESIAN_POINT('',(-2.35933443838445,14.8473002758614,247.086209595194));
#13177=CARTESIAN_POINT('',(-2.44934890711522,14.468701856442,247.086209595194));
#13178=CARTESIAN_POINT('Origin',(-2.35933443838445,14.6473002758614,247.086209595194));
#13179=CARTESIAN_POINT('',(-2.44934890711522,14.468701856442,256.886209595194));
#13180=CARTESIAN_POINT('',(-2.35933443838445,14.8473002758614,256.886209595194));
#13181=CARTESIAN_POINT('Origin',(-2.35933443838447,14.6473002758614,247.086209595194));
#13182=CARTESIAN_POINT('',(-2.35933443838447,14.6473002758614,246.886209595194));
#13183=CARTESIAN_POINT('Origin',(-2.35933443838447,14.6473002758614,247.086209595194));
#13184=CARTESIAN_POINT('Origin',(-2.35933443838447,14.6473002758614,247.086209595194));
#13185=CARTESIAN_POINT('Origin',(-6.5,14.8473002758614,250.657383286513));
#13186=CARTESIAN_POINT('',(3.5,14.8473002758614,250.657383286513));
#13187=CARTESIAN_POINT('',(-6.5,14.8473002758614,250.657383286513));
#13188=CARTESIAN_POINT('',(3.5,14.8473002758614,247.086209595194));
#13189=CARTESIAN_POINT('',(3.5,14.8473002758614,253.771796440853));
#13190=CARTESIAN_POINT('',(-6.5,14.8473002758614,247.086209595194));
#13191=CARTESIAN_POINT('Origin',(-6.5,15.8473002758613,250.657383286513));
#13192=CARTESIAN_POINT('',(3.5,15.0089220887177,251.202472284128));
#13193=CARTESIAN_POINT('',(-6.5,15.0089220887177,251.202472284128));
#13194=CARTESIAN_POINT('Origin',(3.5,15.8473002758613,250.657383286513));
#13195=CARTESIAN_POINT('Origin',(-6.5,16.7024755322828,253.80725475462));
#13196=CARTESIAN_POINT('',(-16.5,15.0089220887177,251.202472284128));
#13197=CARTESIAN_POINT('',(-6.5,15.0089220887177,251.202472284128));
#13198=CARTESIAN_POINT('',(-16.5,16.7024755322828,253.80725475462));
#13199=CARTESIAN_POINT('',(-16.5,14.3945664389275,250.257558007404));
#13200=CARTESIAN_POINT('',(3.5,16.7024755322828,253.80725475462));
#13201=CARTESIAN_POINT('',(-6.5,16.7024755322828,253.80725475462));
#13202=CARTESIAN_POINT('',(3.5,17.3657865921442,254.827465263934));
#13203=CARTESIAN_POINT('Origin',(-6.5,15.8473002758613,250.657383286513));
#13204=CARTESIAN_POINT('',(-16.5,14.8473002758614,250.657383286513));
#13205=CARTESIAN_POINT('',(-6.5,14.8473002758614,250.657383286513));
#13206=CARTESIAN_POINT('Origin',(-16.5,15.8473002758613,250.657383286513));
#13207=CARTESIAN_POINT('Origin',(-6.5,14.8473002758614,250.657383286513));
#13208=CARTESIAN_POINT('',(-16.5,14.8473002758614,247.086209595194));
#13209=CARTESIAN_POINT('',(-6.5,14.8473002758614,247.086209595194));
#13210=CARTESIAN_POINT('',(-16.5,14.8473002758614,253.771796440853));
#13211=CARTESIAN_POINT('Origin',(-6.5,14.6473002758614,247.086209595194));
#13212=CARTESIAN_POINT('',(-16.5,14.6473002758614,246.886209595194));
#13213=CARTESIAN_POINT('',(-6.5,14.6473002758614,246.886209595194));
#13214=CARTESIAN_POINT('Origin',(-16.5,14.6473002758614,247.086209595194));
#13215=CARTESIAN_POINT('Origin',(-6.5,6.43177298256785,247.086209595194));
#13216=CARTESIAN_POINT('',(-15.5,6.43177298256785,247.086209595194));
#13217=CARTESIAN_POINT('Origin',(-6.5,6.43177298256785,247.086209595194));
#13218=CARTESIAN_POINT('',(-10.5506510928848,-1.60515589130626,247.086209595194));
#13219=CARTESIAN_POINT('Origin',(-6.5,6.43177298256785,247.086209595194));
#13220=CARTESIAN_POINT('',(-10.6406655616155,-1.7837543107257,246.886209595194));
#13221=CARTESIAN_POINT('Origin',(-10.6406655616155,-1.7837543107257,247.086209595194));
#13222=CARTESIAN_POINT('Origin',(-6.5,6.43177298256785,246.886209595194));
#13223=CARTESIAN_POINT('Origin',(-2.35933443838448,-1.7837543107257,247.086209595194));
#13224=CARTESIAN_POINT('',(-2.35933443838448,-1.9837543107257,247.086209595194));
#13225=CARTESIAN_POINT('',(-2.44934890711525,-1.60515589130627,247.086209595194));
#13226=CARTESIAN_POINT('Origin',(-2.35933443838448,-1.7837543107257,247.086209595194));
#13227=CARTESIAN_POINT('',(-2.35933443838448,-1.7837543107257,246.886209595194));
#13228=CARTESIAN_POINT('Origin',(-2.35933443838448,-1.7837543107257,247.086209595194));
#13229=CARTESIAN_POINT('Origin',(-2.35933443838448,-1.7837543107257,247.086209595194));
#13230=CARTESIAN_POINT('Origin',(-2.35933443838445,-1.78375431072568,256.886209595194));
#13231=CARTESIAN_POINT('',(-2.35933443838445,-1.98375431072569,250.657383286513));
#13232=CARTESIAN_POINT('',(-2.44934890711523,-1.60515589130626,250.657383286513));
#13233=CARTESIAN_POINT('Origin',(-2.35933443838445,-1.78375431072568,250.657383286513));
#13234=CARTESIAN_POINT('',(-2.44934890711523,-1.60515589130626,256.886209595194));
#13235=CARTESIAN_POINT('',(-2.35933443838445,-1.98375431072568,256.886209595194));
#13236=CARTESIAN_POINT('Ctrl Pts',(-2.35933443838447,-1.98375431072569,
250.657383286513));
#13237=CARTESIAN_POINT('Ctrl Pts',(-2.35933443838446,-1.98375431072569,
250.772822299168));
#13238=CARTESIAN_POINT('Ctrl Pts',(-2.46187926199705,-2.02731361034112,
250.995273610107));
#13239=CARTESIAN_POINT('Ctrl Pts',(-2.66151050029649,-2.10565390596992,
251.141377231877));
#13240=CARTESIAN_POINT('Ctrl Pts',(-2.7689470683364,-2.14537612358201,251.202472284128));
#13241=CARTESIAN_POINT('Ctrl Pts',(-2.4102819870235,-1.98375431072569,250.657383286513));
#13242=CARTESIAN_POINT('Ctrl Pts',(-2.41028198702349,-1.98375431072569,
250.761141960988));
#13243=CARTESIAN_POINT('Ctrl Pts',(-2.50259327156958,-2.01836361311809,
250.965068838285));
#13244=CARTESIAN_POINT('Ctrl Pts',(-2.69407745702402,-2.08894977673007,
251.110832462786));
#13245=CARTESIAN_POINT('Ctrl Pts',(-2.79833310653511,-2.12569665959276,
251.172204138164));
#13246=CARTESIAN_POINT('Ctrl Pts',(-2.51184443386601,-1.94270545541938,
250.657383286513));
#13247=CARTESIAN_POINT('Ctrl Pts',(-2.511844433866,-1.94270545541938,250.742595721283));
#13248=CARTESIAN_POINT('Ctrl Pts',(-2.58378619591607,-1.96368057545467,
250.91832476734));
#13249=CARTESIAN_POINT('Ctrl Pts',(-2.7590798598131,-2.02453104301038,251.06710566137));
#13250=CARTESIAN_POINT('Ctrl Pts',(-2.85696933307462,-2.05794641939893,
251.130326126116));
#13251=CARTESIAN_POINT('Ctrl Pts',(-2.57981436360185,-1.79296837898676,
250.657383286513));
#13252=CARTESIAN_POINT('Ctrl Pts',(-2.57981436360184,-1.79296837898676,
250.74435628427));
#13253=CARTESIAN_POINT('Ctrl Pts',(-2.64258917521035,-1.81562445015628,
250.925879430023));
#13254=CARTESIAN_POINT('Ctrl Pts',(-2.80949734511231,-1.8822863779169,251.084602122621));
#13255=CARTESIAN_POINT('Ctrl Pts',(-2.90391764800065,-1.91879256215878,
251.152000466197));
#13256=CARTESIAN_POINT('Ctrl Pts',(-2.53401156509197,-1.66390087931709,
250.657383286513));
#13257=CARTESIAN_POINT('Ctrl Pts',(-2.53401156509196,-1.66390087931709,
250.769730689184));
#13258=CARTESIAN_POINT('Ctrl Pts',(-2.61306596902394,-1.70195279380099,
250.993661548375));
#13259=CARTESIAN_POINT('Ctrl Pts',(-2.79160486243893,-1.78331601786504,
251.161662294744));
#13260=CARTESIAN_POINT('Ctrl Pts',(-2.89026067918543,-1.82587649606285,
251.232425097961));
#13261=CARTESIAN_POINT('Ctrl Pts',(-2.4720967862658,-1.61662093261596,250.657383286513));
#13262=CARTESIAN_POINT('Ctrl Pts',(-2.4720967862658,-1.61662093261596,250.789388896833));
#13263=CARTESIAN_POINT('Ctrl Pts',(-2.56697742498125,-1.66465600150291,
251.045597335));
#13264=CARTESIAN_POINT('Ctrl Pts',(-2.75789762139033,-1.75418178955874,
251.219068720891));
#13265=CARTESIAN_POINT('Ctrl Pts',(-2.86131674875401,-1.79988152535352,
251.291741549006));
#13266=CARTESIAN_POINT('Ctrl Pts',(-2.44934890711524,-1.60515589130627,
250.657383286513));
#13267=CARTESIAN_POINT('Ctrl Pts',(-2.44934890711524,-1.60515589130626,
250.795910101699));
#13268=CARTESIAN_POINT('Ctrl Pts',(-2.5496644954319,-1.65629072128959,251.062851674826));
#13269=CARTESIAN_POINT('Ctrl Pts',(-2.74495592420308,-1.74825541615818,
251.23817602095));
#13270=CARTESIAN_POINT('Ctrl Pts',(-2.85005691467691,-1.7948858455289,251.311490083651));
#13271=CARTESIAN_POINT('',(-2.7689470683364,-2.14537612358201,251.202472284128));
#13272=CARTESIAN_POINT('',(-2.85005691467691,-1.7948858455289,251.311490083651));
#13273=CARTESIAN_POINT('Origin',(-2.7689470683364,-1.97770048615327,251.311490083651));
#13274=CARTESIAN_POINT('Ctrl Pts',(-2.85005691467691,-1.7948858455289,251.311490083651));
#13275=CARTESIAN_POINT('Ctrl Pts',(-2.74495592420308,-1.74825541615818,
251.23817602095));
#13276=CARTESIAN_POINT('Ctrl Pts',(-2.5496644954319,-1.65629072128959,251.062851674826));
#13277=CARTESIAN_POINT('Ctrl Pts',(-2.44934890711524,-1.60515589130626,
250.795910101699));
#13278=CARTESIAN_POINT('Ctrl Pts',(-2.44934890711524,-1.60515589130627,
250.657383286513));
#13279=CARTESIAN_POINT('Ctrl Pts',(-2.35933443838447,-1.98375431072569,
250.657383286513));
#13280=CARTESIAN_POINT('Ctrl Pts',(-2.35933443838446,-1.98375431072569,
250.772822299168));
#13281=CARTESIAN_POINT('Ctrl Pts',(-2.46187926199705,-2.02731361034112,
250.995273610107));
#13282=CARTESIAN_POINT('Ctrl Pts',(-2.66151050029649,-2.10565390596992,
251.141377231877));
#13283=CARTESIAN_POINT('Ctrl Pts',(-2.7689470683364,-2.14537612358201,251.202472284128));
#13284=CARTESIAN_POINT('Ctrl Pts',(-2.7689470683364,-2.14537612358201,251.202472284128));
#13285=CARTESIAN_POINT('Ctrl Pts',(-3.77226840311965,-2.59052230561913,
251.887132680399));
#13286=CARTESIAN_POINT('Ctrl Pts',(-5.57837183813838,-3.0292444933001,252.561912604368));
#13287=CARTESIAN_POINT('Ctrl Pts',(-8.15338081673582,-2.87490004729592,
252.324521981181));
#13288=CARTESIAN_POINT('Ctrl Pts',(-9.56217204180809,-2.44214024494009,
251.658912548309));
#13289=CARTESIAN_POINT('Ctrl Pts',(-10.2310529316636,-2.14537612358201,
251.202472284128));
#13290=CARTESIAN_POINT('Ctrl Pts',(-2.79833310653511,-2.12569665959276,
251.172204138164));
#13291=CARTESIAN_POINT('Ctrl Pts',(-3.79672716582859,-2.5678363253453,251.852198827549));
#13292=CARTESIAN_POINT('Ctrl Pts',(-5.58802871625117,-3.00150512886098,
252.519153595767));
#13293=CARTESIAN_POINT('Ctrl Pts',(-8.13659337144744,-2.84912459574666,
252.284803763196));
#13294=CARTESIAN_POINT('Ctrl Pts',(-9.53607085393589,-2.42045643676112,
251.625533931087));
#13295=CARTESIAN_POINT('Ctrl Pts',(-10.2016668934649,-2.12569665959276,
251.172204138164));
#13296=CARTESIAN_POINT('Ctrl Pts',(-2.85696935144547,-2.05794617860782,
251.13032625575));
#13297=CARTESIAN_POINT('Ctrl Pts',(-3.84550834632558,-2.49248211993982,
251.802015209738));
#13298=CARTESIAN_POINT('Ctrl Pts',(-5.60737730602117,-2.91405769435918,
252.454604565079));
#13299=CARTESIAN_POINT('Ctrl Pts',(-8.10304493491812,-2.76633681628283,
252.225863919145));
#13300=CARTESIAN_POINT('Ctrl Pts',(-9.48400465196778,-2.34763680616248,
251.578118891742));
#13301=CARTESIAN_POINT('Ctrl Pts',(-10.1430306485545,-2.05794617860782,
251.13032625575));
#13302=CARTESIAN_POINT('Ctrl Pts',(-2.90391767111428,-1.91879244249013,
251.152000510131));
#13303=CARTESIAN_POINT('Ctrl Pts',(-3.88254920604482,-2.34506924067967,
251.82148239871));
#13304=CARTESIAN_POINT('Ctrl Pts',(-5.62105275595405,-2.75575651795704,
252.469871929561));
#13305=CARTESIAN_POINT('Ctrl Pts',(-8.07893705070351,-2.61209324920213,
252.242793964634));
#13306=CARTESIAN_POINT('Ctrl Pts',(-9.44366130559868,-2.2029769746165,251.598321769183));
#13307=CARTESIAN_POINT('Ctrl Pts',(-10.0960823288857,-1.91879244249013,
251.152000510131));
#13308=CARTESIAN_POINT('Ctrl Pts',(-2.89026069830919,-1.82587639593774,
251.232425135035));
#13309=CARTESIAN_POINT('Ctrl Pts',(-3.86765930897934,-2.2537442325047,251.90907507138));
#13310=CARTESIAN_POINT('Ctrl Pts',(-5.61370506773033,-2.66971313360356,
252.569860268798));
#13311=CARTESIAN_POINT('Ctrl Pts',(-8.09123862855148,-2.52386111525648,
252.33794267841));
#13312=CARTESIAN_POINT('Ctrl Pts',(-9.4581402279107,-2.11112162031572,251.683525092599));
#13313=CARTESIAN_POINT('Ctrl Pts',(-10.1097393016908,-1.82587639593775,
251.232425135035));
#13314=CARTESIAN_POINT('Ctrl Pts',(-2.86131674875401,-1.79988152535352,
251.291741549006));
#13315=CARTESIAN_POINT('Ctrl Pts',(-3.84154141667882,-2.23319023011266,
251.97440989295));
#13316=CARTESIAN_POINT('Ctrl Pts',(-5.60252881155338,-2.65875979334497,
252.645711029322));
#13317=CARTESIAN_POINT('Ctrl Pts',(-8.11031912498652,-2.50916768931843,
252.40968064353));
#13318=CARTESIAN_POINT('Ctrl Pts',(-9.48520013929611,-2.08875399519296,
251.746853778302));
#13319=CARTESIAN_POINT('Ctrl Pts',(-10.138683251246,-1.79988152535353,251.291741549006));
#13320=CARTESIAN_POINT('Ctrl Pts',(-2.85005691467691,-1.7948858455289,251.311490083651));
#13321=CARTESIAN_POINT('Ctrl Pts',(-3.83156691609531,-2.23035493665217,
251.996150479922));
#13322=CARTESIAN_POINT('Ctrl Pts',(-5.59840723296145,-2.65953968547052,
252.670930403891));
#13323=CARTESIAN_POINT('Ctrl Pts',(-8.11743775550243,-2.5085505535099,252.433539780704));
#13324=CARTESIAN_POINT('Ctrl Pts',(-9.49560308437748,-2.08519857294442,
251.767930347832));
#13325=CARTESIAN_POINT('Ctrl Pts',(-10.1499430853231,-1.79488584552891,
251.311490083651));
#13326=CARTESIAN_POINT('',(-10.2310529316636,-2.14537612358201,251.202472284128));
#13327=CARTESIAN_POINT('',(-10.1499430853231,-1.79488584552891,251.311490083651));
#13328=CARTESIAN_POINT('Origin',(-10.2310529316636,-1.97770048615328,251.311490083651));
#13329=CARTESIAN_POINT('Origin',(-6.5,6.43177298256785,238.377236865592));
#13330=CARTESIAN_POINT('Origin',(-6.5,6.26409734513912,238.268219066069));
#13331=CARTESIAN_POINT('Ctrl Pts',(-10.2310529316636,-2.14537612358201,
251.202472284128));
#13332=CARTESIAN_POINT('Ctrl Pts',(-10.3384971542717,-2.10565107586813,
251.141372879018));
#13333=CARTESIAN_POINT('Ctrl Pts',(-10.5381140246013,-2.02731718901882,
250.995305028042));
#13334=CARTESIAN_POINT('Ctrl Pts',(-10.6406655616155,-1.98375431072569,
250.772830523889));
#13335=CARTESIAN_POINT('Ctrl Pts',(-10.6406655616155,-1.98375431072569,
250.657383286513));
#13336=CARTESIAN_POINT('Ctrl Pts',(-10.2016668934649,-2.12569665959276,
251.172204138164));
#13337=CARTESIAN_POINT('Ctrl Pts',(-10.3059299709122,-2.08894715861293,
251.110828090218));
#13338=CARTESIAN_POINT('Ctrl Pts',(-10.4974012709103,-2.01836605599956,
250.965097544891));
#13339=CARTESIAN_POINT('Ctrl Pts',(-10.5897180129765,-1.98375431072569,
250.761149353516));
#13340=CARTESIAN_POINT('Ctrl Pts',(-10.5897180129765,-1.98375431072569,
250.657383286513));
#13341=CARTESIAN_POINT('Ctrl Pts',(-10.1430306485535,-2.05794617859384,
251.130326255758));
#13342=CARTESIAN_POINT('Ctrl Pts',(-10.2409270961782,-2.02452842144907,
251.067101286723));
#13343=CARTESIAN_POINT('Ctrl Pts',(-10.4162108293298,-1.96368091150233,
250.918349437673));
#13344=CARTESIAN_POINT('Ctrl Pts',(-10.4881555222276,-1.94270505090509,
250.742601792441));
#13345=CARTESIAN_POINT('Ctrl Pts',(-10.4881555222275,-1.94270505090509,
250.657383286512));
#13346=CARTESIAN_POINT('Ctrl Pts',(-10.0960823288844,-1.91879244248318,
251.152000510133));
#13347=CARTESIAN_POINT('Ctrl Pts',(-10.1905093589668,-1.88228365727328,
251.084597364605));
#13348=CARTESIAN_POINT('Ctrl Pts',(-10.3574089229965,-1.8156250085404,250.925904890041));
#13349=CARTESIAN_POINT('Ctrl Pts',(-10.4201855817356,-1.79296819025683,
250.744362480863));
#13350=CARTESIAN_POINT('Ctrl Pts',(-10.4201855817356,-1.79296819025684,
250.657383286513));
#13351=CARTESIAN_POINT('Ctrl Pts',(-10.1097393016897,-1.82587639593193,
251.232425135037));
#13352=CARTESIAN_POINT('Ctrl Pts',(-10.2084021473994,-1.78331288541385,
251.16165729016));
#13353=CARTESIAN_POINT('Ctrl Pts',(-10.3869300787649,-1.70195523407075,
250.993693094235));
#13354=CARTESIAN_POINT('Ctrl Pts',(-10.4659883891908,-1.66390072133625,
250.769738693635));
#13355=CARTESIAN_POINT('Ctrl Pts',(-10.4659883891907,-1.66390072133626,
250.657383286512));
#13356=CARTESIAN_POINT('Ctrl Pts',(-10.138683251246,-1.79988152535352,251.291741549006));
#13357=CARTESIAN_POINT('Ctrl Pts',(-10.242109746946,-1.75417853357476,251.219063543146));
#13358=CARTESIAN_POINT('Ctrl Pts',(-10.4330166775059,-1.66465981113938,
251.04563349778));
#13359=CARTESIAN_POINT('Ctrl Pts',(-10.5279032137342,-1.61662093261595,
250.789398301879));
#13360=CARTESIAN_POINT('Ctrl Pts',(-10.5279032137342,-1.61662093261596,
250.657383286513));
#13361=CARTESIAN_POINT('Ctrl Pts',(-10.1499430853231,-1.7948858455289,251.311490083651));
#13362=CARTESIAN_POINT('Ctrl Pts',(-10.2550515639615,-1.74825209386477,
251.238170797519));
#13363=CARTESIAN_POINT('Ctrl Pts',(-10.45032893711,-1.65629492234602,251.062889376348));
#13364=CARTESIAN_POINT('Ctrl Pts',(-10.5506510928848,-1.60515589130626,
250.795919971364));
#13365=CARTESIAN_POINT('Ctrl Pts',(-10.5506510928848,-1.60515589130627,
250.657383286513));
#13366=CARTESIAN_POINT('',(-10.6406655616155,-1.98375431072569,250.657383286513));
#13367=CARTESIAN_POINT('',(-10.5506510928848,-1.60515589130627,250.657383286513));
#13368=CARTESIAN_POINT('Origin',(-10.6406655616155,-1.78375431072569,250.657383286513));
#13369=CARTESIAN_POINT('Ctrl Pts',(-10.5506510928848,-1.60515589130627,
250.657383286513));
#13370=CARTESIAN_POINT('Ctrl Pts',(-10.5506510928848,-1.60515589130626,
250.795919971364));
#13371=CARTESIAN_POINT('Ctrl Pts',(-10.45032893711,-1.65629492234602,251.062889376348));
#13372=CARTESIAN_POINT('Ctrl Pts',(-10.2550515639615,-1.74825209386477,
251.238170797519));
#13373=CARTESIAN_POINT('Ctrl Pts',(-10.1499430853231,-1.7948858455289,251.311490083651));
#13374=CARTESIAN_POINT('Ctrl Pts',(-10.2310529316636,-2.14537612358201,
251.202472284128));
#13375=CARTESIAN_POINT('Ctrl Pts',(-10.3384971542717,-2.10565107586813,
251.141372879018));
#13376=CARTESIAN_POINT('Ctrl Pts',(-10.5381140246013,-2.02731718901882,
250.995305028042));
#13377=CARTESIAN_POINT('Ctrl Pts',(-10.6406655616155,-1.98375431072569,
250.772830523889));
#13378=CARTESIAN_POINT('Ctrl Pts',(-10.6406655616155,-1.98375431072569,
250.657383286513));
#13379=CARTESIAN_POINT('Origin',(-10.6406655616155,-1.78375431072568,256.886209595194));
#13380=CARTESIAN_POINT('',(-10.6406655616155,-1.9837543107257,247.086209595194));
#13381=CARTESIAN_POINT('Origin',(-10.6406655616155,-1.78375431072568,247.086209595194));
#13382=CARTESIAN_POINT('',(-10.5506510928848,-1.60515589130626,256.886209595194));
#13383=CARTESIAN_POINT('',(-10.6406655616155,-1.98375431072568,256.886209595194));
#13384=CARTESIAN_POINT('Origin',(-10.6406655616155,-1.7837543107257,247.086209595194));
#13385=CARTESIAN_POINT('Origin',(-10.6406655616155,-1.7837543107257,247.086209595194));
#13386=CARTESIAN_POINT('Origin',(-6.5,-1.9837543107257,246.886209595194));
#13387=CARTESIAN_POINT('',(-16.5,-1.98375431072569,250.657383286513));
#13388=CARTESIAN_POINT('',(-6.5,-1.98375431072569,250.657383286513));
#13389=CARTESIAN_POINT('',(-16.5,-1.9837543107257,247.086209595194));
#13390=CARTESIAN_POINT('',(-16.5,-1.98375431072569,251.886209595194));
#13391=CARTESIAN_POINT('',(-6.5,-1.9837543107257,247.086209595194));
#13392=CARTESIAN_POINT('Origin',(-6.5,-2.98375431072556,250.657383286513));
#13393=CARTESIAN_POINT('',(-16.5,-2.14537612358201,251.202472284128));
#13394=CARTESIAN_POINT('',(-6.5,-2.14537612358201,251.202472284128));
#13395=CARTESIAN_POINT('Origin',(-16.5,-2.98375431072556,250.657383286513));
#13396=CARTESIAN_POINT('Origin',(-6.5,-2.14537612358201,251.202472284128));
#13397=CARTESIAN_POINT('',(3.5,-2.14537612358201,251.202472284128));
#13398=CARTESIAN_POINT('',(-6.5,-2.14537612358201,251.202472284128));
#13399=CARTESIAN_POINT('',(3.5,-3.83892956714709,253.80725475462));
#13400=CARTESIAN_POINT('',(3.5,-0.684243752009264,248.955166772158));
#13401=CARTESIAN_POINT('',(-16.5,-3.83892956714709,253.80725475462));
#13402=CARTESIAN_POINT('',(-6.5,-3.83892956714709,253.80725475462));
#13403=CARTESIAN_POINT('',(-16.5,-3.65546390522595,253.525074028688));
#13404=CARTESIAN_POINT('Origin',(-6.5,-2.98375431072556,250.657383286513));
#13405=CARTESIAN_POINT('',(3.5,-1.98375431072569,250.657383286513));
#13406=CARTESIAN_POINT('',(-6.5,-1.98375431072569,250.657383286513));
#13407=CARTESIAN_POINT('Origin',(3.5,-2.98375431072556,250.657383286513));
#13408=CARTESIAN_POINT('Origin',(-6.5,-1.9837543107257,246.886209595194));
#13409=CARTESIAN_POINT('',(3.5,-1.9837543107257,247.086209595194));
#13410=CARTESIAN_POINT('',(-6.5,-1.9837543107257,247.086209595194));
#13411=CARTESIAN_POINT('',(3.5,-1.98375431072569,251.886209595194));
#13412=CARTESIAN_POINT('Origin',(-6.5,-1.7837543107257,247.086209595194));
#13413=CARTESIAN_POINT('',(3.5,-1.7837543107257,246.886209595194));
#13414=CARTESIAN_POINT('',(-6.5,-1.7837543107257,246.886209595194));
#13415=CARTESIAN_POINT('Origin',(3.5,-1.7837543107257,247.086209595194));
#13416=CARTESIAN_POINT('Origin',(-6.5,6.43177298256785,247.086209595194));
#13417=CARTESIAN_POINT('Origin',(-6.5,6.43177298256785,246.886209595194));
#13418=CARTESIAN_POINT('Origin',(-6.5,6.43177298256785,247.086209595194));
#13419=CARTESIAN_POINT('Origin',(-6.5,14.6473002758614,247.086209595194));
#13420=CARTESIAN_POINT('',(3.5,14.6473002758614,246.886209595194));
#13421=CARTESIAN_POINT('Origin',(3.5,14.6473002758614,247.086209595194));
#13422=CARTESIAN_POINT('',(-6.5,14.6473002758614,246.886209595194));
#13423=CARTESIAN_POINT('Ctrl Pts',(3.7,14.4473002758614,246.886209595194));
#13424=CARTESIAN_POINT('Ctrl Pts',(3.7,14.6473002758614,246.886209595194));
#13425=CARTESIAN_POINT('Ctrl Pts',(3.5,14.6473002758614,246.886209595194));
#13426=CARTESIAN_POINT('Ctrl Pts',(3.90000000000004,14.4473002758614,246.886209595194));
#13427=CARTESIAN_POINT('Ctrl Pts',(3.90000000000004,14.8473002758614,246.886209595194));
#13428=CARTESIAN_POINT('Ctrl Pts',(3.5,14.8473002758614,246.886209595194));
#13429=CARTESIAN_POINT('Ctrl Pts',(3.9,14.4473002758614,247.086209595194));
#13430=CARTESIAN_POINT('Ctrl Pts',(3.9,14.8473002758614,247.086209595194));
#13431=CARTESIAN_POINT('Ctrl Pts',(3.5,14.8473002758614,247.086209595194));
#13432=CARTESIAN_POINT('',(3.9,14.4473002758614,247.086209595194));
#13433=CARTESIAN_POINT('',(3.7,14.4473002758614,246.886209595194));
#13434=CARTESIAN_POINT('Origin',(3.7,14.4473002758614,247.086209595194));
#13435=CARTESIAN_POINT('Origin',(3.5,14.4473002758614,246.886209595194));
#13436=CARTESIAN_POINT('Origin',(3.5,14.4473002758614,247.086209595194));
#13437=CARTESIAN_POINT('Origin',(3.7,11.4317729825679,247.086209595194));
#13438=CARTESIAN_POINT('',(3.9,-1.5837543107257,247.086209595194));
#13439=CARTESIAN_POINT('',(3.7,-1.5837543107257,246.886209595194));
#13440=CARTESIAN_POINT('Origin',(3.7,-1.5837543107257,247.086209595194));
#13441=CARTESIAN_POINT('',(3.7,11.4317729825679,246.886209595194));
#13442=CARTESIAN_POINT('',(3.9,11.4317729825679,247.086209595194));
#13443=CARTESIAN_POINT('Ctrl Pts',(3.5,-1.7837543107257,246.886209595194));
#13444=CARTESIAN_POINT('Ctrl Pts',(3.7,-1.7837543107257,246.886209595194));
#13445=CARTESIAN_POINT('Ctrl Pts',(3.7,-1.5837543107257,246.886209595194));
#13446=CARTESIAN_POINT('Ctrl Pts',(3.5,-1.9837543107257,246.886209595194));
#13447=CARTESIAN_POINT('Ctrl Pts',(3.9,-1.9837543107257,246.886209595194));
#13448=CARTESIAN_POINT('Ctrl Pts',(3.9,-1.5837543107257,246.886209595194));
#13449=CARTESIAN_POINT('Ctrl Pts',(3.5,-1.9837543107257,247.086209595194));
#13450=CARTESIAN_POINT('Ctrl Pts',(3.9,-1.9837543107257,247.086209595194));
#13451=CARTESIAN_POINT('Ctrl Pts',(3.9,-1.5837543107257,247.086209595194));
#13452=CARTESIAN_POINT('Origin',(3.5,-1.5837543107257,246.886209595194));
#13453=CARTESIAN_POINT('Origin',(3.5,-1.5837543107257,247.086209595194));
#13454=CARTESIAN_POINT('Origin',(3.5,14.4473002758614,253.771796440853));
#13455=CARTESIAN_POINT('',(3.9,14.4473002758614,250.657383286513));
#13456=CARTESIAN_POINT('Origin',(3.5,14.4473002758614,250.657383286513));
#13457=CARTESIAN_POINT('',(3.9,14.4473002758614,253.771796440853));
#13458=CARTESIAN_POINT('Origin',(-6.5,6.43177298256785,256.886209595194));
#13459=CARTESIAN_POINT('',(-15.5,6.43177298256785,256.886209595194));
#13460=CARTESIAN_POINT('Origin',(-6.5,6.43177298256785,246.886209595194));
#13461=CARTESIAN_POINT('Origin',(-6.5,-1.7837543107257,247.086209595194));
#13462=CARTESIAN_POINT('',(-16.5,-1.7837543107257,246.886209595194));
#13463=CARTESIAN_POINT('Origin',(-16.5,-1.7837543107257,247.086209595194));
#13464=CARTESIAN_POINT('',(-6.5,-1.7837543107257,246.886209595194));
#13465=CARTESIAN_POINT('Ctrl Pts',(-16.7,-1.5837543107257,246.886209595194));
#13466=CARTESIAN_POINT('Ctrl Pts',(-16.7,-1.7837543107257,246.886209595194));
#13467=CARTESIAN_POINT('Ctrl Pts',(-16.5,-1.7837543107257,246.886209595194));
#13468=CARTESIAN_POINT('Ctrl Pts',(-16.9,-1.5837543107257,246.886209595194));
#13469=CARTESIAN_POINT('Ctrl Pts',(-16.9,-1.9837543107257,246.886209595194));
#13470=CARTESIAN_POINT('Ctrl Pts',(-16.5,-1.9837543107257,246.886209595194));
#13471=CARTESIAN_POINT('Ctrl Pts',(-16.9,-1.5837543107257,247.086209595194));
#13472=CARTESIAN_POINT('Ctrl Pts',(-16.9,-1.9837543107257,247.086209595194));
#13473=CARTESIAN_POINT('Ctrl Pts',(-16.5,-1.9837543107257,247.086209595194));
#13474=CARTESIAN_POINT('',(-16.9,-1.5837543107257,247.086209595194));
#13475=CARTESIAN_POINT('',(-16.7,-1.5837543107257,246.886209595194));
#13476=CARTESIAN_POINT('Origin',(-16.7,-1.5837543107257,247.086209595194));
#13477=CARTESIAN_POINT('Origin',(-16.5,-1.5837543107257,246.886209595194));
#13478=CARTESIAN_POINT('Origin',(-16.5,-1.5837543107257,247.086209595194));
#13479=CARTESIAN_POINT('Origin',(-16.7,1.43177298256785,247.086209595194));
#13480=CARTESIAN_POINT('',(-16.9,14.4473002758614,247.086209595194));
#13481=CARTESIAN_POINT('',(-16.7,14.4473002758614,246.886209595194));
#13482=CARTESIAN_POINT('Origin',(-16.7,14.4473002758614,247.086209595194));
#13483=CARTESIAN_POINT('',(-16.7,1.43177298256785,246.886209595194));
#13484=CARTESIAN_POINT('',(-16.9,1.43177298256785,247.086209595194));
#13485=CARTESIAN_POINT('Ctrl Pts',(-16.5,14.6473002758614,246.886209595194));
#13486=CARTESIAN_POINT('Ctrl Pts',(-16.7,14.6473002758614,246.886209595194));
#13487=CARTESIAN_POINT('Ctrl Pts',(-16.7,14.4473002758614,246.886209595194));
#13488=CARTESIAN_POINT('Ctrl Pts',(-16.5,14.8473002758614,246.886209595194));
#13489=CARTESIAN_POINT('Ctrl Pts',(-16.9,14.8473002758614,246.886209595194));
#13490=CARTESIAN_POINT('Ctrl Pts',(-16.9,14.4473002758614,246.886209595194));
#13491=CARTESIAN_POINT('Ctrl Pts',(-16.5,14.8473002758614,247.086209595194));
#13492=CARTESIAN_POINT('Ctrl Pts',(-16.9,14.8473002758614,247.086209595194));
#13493=CARTESIAN_POINT('Ctrl Pts',(-16.9,14.4473002758614,247.086209595194));
#13494=CARTESIAN_POINT('Origin',(-16.5,14.4473002758614,246.886209595194));
#13495=CARTESIAN_POINT('Origin',(-16.5,14.4473002758614,247.086209595194));
#13496=CARTESIAN_POINT('Origin',(-16.5,-1.58375431072569,251.886209595194));
#13497=CARTESIAN_POINT('',(-16.9,-1.58375431072569,250.657383286513));
#13498=CARTESIAN_POINT('Origin',(-16.5,-1.58375431072569,250.657383286513));
#13499=CARTESIAN_POINT('',(-16.9,-1.58375431072569,251.886209595194));
#13500=CARTESIAN_POINT('Origin',(-6.5,6.43177298256785,246.886209595194));
#13501=CARTESIAN_POINT('Origin',(3.5,-0.348892477151795,249.173202371204));
#13502=CARTESIAN_POINT('',(3.9,-3.50357829228962,254.025290353666));
#13503=CARTESIAN_POINT('Origin',(3.5,-3.50357829228962,254.025290353666));
#13504=CARTESIAN_POINT('',(3.9,-1.81002484872454,251.420507883174));
#13505=CARTESIAN_POINT('Origin',(3.5,-1.81002484872454,251.420507883174));
#13506=CARTESIAN_POINT('',(3.9,-0.348892477151795,249.173202371204));
#13507=CARTESIAN_POINT('Origin',(3.5,-2.98375431072556,250.657383286513));
#13508=CARTESIAN_POINT('',(3.9,-1.58375431072569,250.657383286513));
#13509=CARTESIAN_POINT('Origin',(3.5,-1.58375431072569,250.657383286513));
#13510=CARTESIAN_POINT('Origin',(3.9,-2.98375431072556,250.657383286513));
#13511=CARTESIAN_POINT('Origin',(3.5,-1.58375431072569,251.886209595194));
#13512=CARTESIAN_POINT('',(3.9,-1.58375431072569,251.886209595194));
#13513=CARTESIAN_POINT('Ctrl Pts',(3.5,-3.96822701743216,254.243325952712));
#13514=CARTESIAN_POINT('Ctrl Pts',(3.5,-3.96822701743216,254.006121659742));
#13515=CARTESIAN_POINT('Ctrl Pts',(3.5,-3.83892956714706,253.80725475462));
#13516=CARTESIAN_POINT('Ctrl Pts',(3.90000000000001,-3.96822701743216,254.243325952712));
#13517=CARTESIAN_POINT('Ctrl Pts',(3.90000000000001,-3.96822701743216,254.006121659742));
#13518=CARTESIAN_POINT('Ctrl Pts',(3.90000000000001,-3.83892956714706,253.80725475462));
#13519=CARTESIAN_POINT('Ctrl Pts',(3.9,-3.56822701743216,254.243325952712));
#13520=CARTESIAN_POINT('Ctrl Pts',(3.9,-3.56822701743216,254.124723806227));
#13521=CARTESIAN_POINT('Ctrl Pts',(3.9,-3.50357829228961,254.025290353666));
#13522=CARTESIAN_POINT('',(3.9,-3.56822701743215,254.243325952712));
#13523=CARTESIAN_POINT('',(3.5,-3.96822701743215,254.243325952712));
#13524=CARTESIAN_POINT('Origin',(3.5,-3.56822701743216,254.243325952712));
#13525=CARTESIAN_POINT('Origin',(3.5,-3.1682270174321,254.243325952712));
#13526=CARTESIAN_POINT('Origin',(3.9,-3.1682270174321,254.243325952712));
#13527=CARTESIAN_POINT('Origin',(3.9,16.4317729825679,256.886209595194));
#13528=CARTESIAN_POINT('',(3.9,14.6735708138602,251.420507883175));
#13529=CARTESIAN_POINT('Origin',(3.9,15.8473002758613,250.657383286513));
#13530=CARTESIAN_POINT('',(3.9,16.3671242574253,254.025290353666));
#13531=CARTESIAN_POINT('',(3.9,17.0304353172867,255.04550086298));
#13532=CARTESIAN_POINT('',(3.9,16.4317729825679,254.243325952712));
#13533=CARTESIAN_POINT('Origin',(3.9,16.0317729825678,254.243325952712));
#13534=CARTESIAN_POINT('',(3.9,16.4317729825679,256.886209595194));
#13535=CARTESIAN_POINT('',(3.9,16.4317729825679,256.886209595194));
#13536=CARTESIAN_POINT('',(3.9,-3.56822701743215,256.886209595194));
#13537=CARTESIAN_POINT('',(3.9,11.4317729825679,256.886209595194));
#13538=CARTESIAN_POINT('',(3.9,-3.56822701743215,256.886209595194));
#13539=CARTESIAN_POINT('',(3.9,4.64187227009995,247.547898263196));
#13540=CARTESIAN_POINT('',(3.9,8.22167369503577,247.547898263196));
#13541=CARTESIAN_POINT('Origin',(3.9,6.43177298256785,249.937669285906));
#13542=CARTESIAN_POINT('',(3.9,10.5368226263339,247.547898263195));
#13543=CARTESIAN_POINT('Origin',(3.5,15.8473002758613,250.657383286513));
#13544=CARTESIAN_POINT('Origin',(3.5,14.6735708138602,251.420507883175));
#13545=CARTESIAN_POINT('Origin',(3.5,17.0304353172867,255.04550086298));
#13546=CARTESIAN_POINT('Origin',(3.5,16.3671242574253,254.025290353666));
#13547=CARTESIAN_POINT('Ctrl Pts',(3.5,16.7024755322828,253.80725475462));
#13548=CARTESIAN_POINT('Ctrl Pts',(3.5,16.8317729825679,254.006121659742));
#13549=CARTESIAN_POINT('Ctrl Pts',(3.5,16.8317729825679,254.243325952712));
#13550=CARTESIAN_POINT('Ctrl Pts',(3.9,16.7024755322828,253.80725475462));
#13551=CARTESIAN_POINT('Ctrl Pts',(3.9,16.8317729825679,254.006121659742));
#13552=CARTESIAN_POINT('Ctrl Pts',(3.9,16.8317729825679,254.243325952712));
#13553=CARTESIAN_POINT('Ctrl Pts',(3.9,16.3671242574253,254.025290353666));
#13554=CARTESIAN_POINT('Ctrl Pts',(3.9,16.4317729825679,254.124723806227));
#13555=CARTESIAN_POINT('Ctrl Pts',(3.9,16.4317729825679,254.243325952712));
#13556=CARTESIAN_POINT('',(3.5,16.8317729825679,254.243325952712));
#13557=CARTESIAN_POINT('Origin',(3.5,16.4317729825679,254.243325952712));
#13558=CARTESIAN_POINT('Origin',(3.5,16.0317729825678,254.243325952712));
#13559=CARTESIAN_POINT('Origin',(-16.5,14.05921516407,250.47559360645));
#13560=CARTESIAN_POINT('',(-16.9,16.3671242574253,254.025290353666));
#13561=CARTESIAN_POINT('Origin',(-16.5,16.3671242574253,254.025290353666));
#13562=CARTESIAN_POINT('',(-16.9,14.6735708138602,251.420507883174));
#13563=CARTESIAN_POINT('Origin',(-16.5,14.6735708138602,251.420507883174));
#13564=CARTESIAN_POINT('',(-16.9,14.05921516407,250.47559360645));
#13565=CARTESIAN_POINT('Origin',(-16.5,15.8473002758613,250.657383286513));
#13566=CARTESIAN_POINT('',(-16.9,14.4473002758614,250.657383286513));
#13567=CARTESIAN_POINT('Origin',(-16.5,14.4473002758614,250.657383286513));
#13568=CARTESIAN_POINT('Origin',(-16.9,15.8473002758613,250.657383286513));
#13569=CARTESIAN_POINT('Origin',(-16.5,14.4473002758614,253.771796440853));
#13570=CARTESIAN_POINT('',(-16.9,14.4473002758614,253.771796440853));
#13571=CARTESIAN_POINT('Ctrl Pts',(-16.5,16.8317729825679,254.243325952712));
#13572=CARTESIAN_POINT('Ctrl Pts',(-16.5,16.8317729825679,254.006121659742));
#13573=CARTESIAN_POINT('Ctrl Pts',(-16.5,16.7024755322828,253.80725475462));
#13574=CARTESIAN_POINT('Ctrl Pts',(-16.9,16.8317729825679,254.243325952712));
#13575=CARTESIAN_POINT('Ctrl Pts',(-16.9,16.8317729825679,254.006121659742));
#13576=CARTESIAN_POINT('Ctrl Pts',(-16.9,16.7024755322828,253.80725475462));
#13577=CARTESIAN_POINT('Ctrl Pts',(-16.9,16.4317729825679,254.243325952712));
#13578=CARTESIAN_POINT('Ctrl Pts',(-16.9,16.4317729825679,254.124723806227));
#13579=CARTESIAN_POINT('Ctrl Pts',(-16.9,16.3671242574253,254.025290353666));
#13580=CARTESIAN_POINT('',(-16.9,16.4317729825678,254.243325952712));
#13581=CARTESIAN_POINT('',(-16.5,16.8317729825679,254.243325952712));
#13582=CARTESIAN_POINT('Origin',(-16.5,16.4317729825679,254.243325952712));
#13583=CARTESIAN_POINT('Origin',(-16.5,16.0317729825678,254.243325952712));
#13584=CARTESIAN_POINT('Origin',(-16.9,16.0317729825678,254.243325952712));
#13585=CARTESIAN_POINT('Origin',(-16.9,-3.56822701743215,256.886209595194));
#13586=CARTESIAN_POINT('',(-16.9,-1.81002484872455,251.420507883175));
#13587=CARTESIAN_POINT('Origin',(-16.9,-2.98375431072556,250.657383286513));
#13588=CARTESIAN_POINT('',(-16.9,-3.50357829228962,254.025290353666));
#13589=CARTESIAN_POINT('',(-16.9,-3.32011263036848,253.743109627734));
#13590=CARTESIAN_POINT('',(-16.9,-3.56822701743215,254.243325952712));
#13591=CARTESIAN_POINT('Origin',(-16.9,-3.1682270174321,254.243325952712));
#13592=CARTESIAN_POINT('',(-16.9,-3.56822701743215,256.886209595194));
#13593=CARTESIAN_POINT('',(-16.9,-3.56822701743215,256.886209595194));
#13594=CARTESIAN_POINT('',(-16.9,16.4317729825678,256.886209595194));
#13595=CARTESIAN_POINT('',(-16.9,1.43177298256785,256.886209595194));
#13596=CARTESIAN_POINT('',(-16.9,16.4317729825678,256.886209595194));
#13597=CARTESIAN_POINT('',(-16.9,4.64187227009995,247.547898263196));
#13598=CARTESIAN_POINT('',(-16.9,8.22167369503577,247.547898263196));
#13599=CARTESIAN_POINT('',(-16.9,0.536822626333899,247.547898263195));
#13600=CARTESIAN_POINT('Origin',(-16.9,6.43177298256785,249.937669285906));
#13601=CARTESIAN_POINT('Origin',(-16.5,-2.98375431072556,250.657383286513));
#13602=CARTESIAN_POINT('Origin',(-16.5,-1.81002484872455,251.420507883175));
#13603=CARTESIAN_POINT('Origin',(-16.5,-3.32011263036848,253.743109627734));
#13604=CARTESIAN_POINT('Origin',(-16.5,-3.50357829228962,254.025290353666));
#13605=CARTESIAN_POINT('Ctrl Pts',(-16.5,-3.83892956714706,253.80725475462));
#13606=CARTESIAN_POINT('Ctrl Pts',(-16.5,-3.96822701743216,254.006121659742));
#13607=CARTESIAN_POINT('Ctrl Pts',(-16.5,-3.96822701743216,254.243325952712));
#13608=CARTESIAN_POINT('Ctrl Pts',(-16.9,-3.83892956714706,253.80725475462));
#13609=CARTESIAN_POINT('Ctrl Pts',(-16.9,-3.96822701743216,254.006121659742));
#13610=CARTESIAN_POINT('Ctrl Pts',(-16.9,-3.96822701743216,254.243325952712));
#13611=CARTESIAN_POINT('Ctrl Pts',(-16.9,-3.50357829228961,254.025290353666));
#13612=CARTESIAN_POINT('Ctrl Pts',(-16.9,-3.56822701743216,254.124723806227));
#13613=CARTESIAN_POINT('Ctrl Pts',(-16.9,-3.56822701743216,254.243325952712));
#13614=CARTESIAN_POINT('',(-16.5,-3.96822701743215,254.243325952712));
#13615=CARTESIAN_POINT('Origin',(-16.5,-3.56822701743216,254.243325952712));
#13616=CARTESIAN_POINT('Origin',(-16.5,-3.1682270174321,254.243325952712));
#13617=CARTESIAN_POINT('Origin',(-6.5,16.0317729825678,254.243325952712));
#13618=CARTESIAN_POINT('',(-6.5,16.8317729825679,254.243325952712));
#13619=CARTESIAN_POINT('Origin',(-6.5,-3.1682270174321,254.243325952712));
#13620=CARTESIAN_POINT('',(-6.5,-3.96822701743215,254.243325952712));
#13621=CARTESIAN_POINT('Origin',(-16.5,16.8317729825679,256.886209595194));
#13622=CARTESIAN_POINT('',(-16.5,16.8317729825679,256.886209595194));
#13623=CARTESIAN_POINT('',(-16.5,16.8317729825679,256.886209595194));
#13624=CARTESIAN_POINT('',(3.5,16.8317729825679,256.886209595194));
#13625=CARTESIAN_POINT('',(-11.5,16.8317729825679,256.886209595194));
#13626=CARTESIAN_POINT('',(3.5,16.8317729825679,256.886209595194));
#13627=CARTESIAN_POINT('Origin',(3.5,-3.96822701743215,256.886209595194));
#13628=CARTESIAN_POINT('',(3.5,-3.96822701743215,256.886209595194));
#13629=CARTESIAN_POINT('',(3.5,-3.96822701743215,256.886209595194));
#13630=CARTESIAN_POINT('',(-16.5,-3.96822701743215,256.886209595194));
#13631=CARTESIAN_POINT('',(-1.5,-3.96822701743215,256.886209595194));
#13632=CARTESIAN_POINT('',(-16.5,-3.96822701743215,256.886209595194));
#13633=CARTESIAN_POINT('Origin',(-6.5,6.43177298256785,249.937669285906));
#13634=CARTESIAN_POINT('',(5.5,4.64187227009995,247.547898263196));
#13635=CARTESIAN_POINT('',(-6.5,4.64187227009995,247.547898263196));
#13636=CARTESIAN_POINT('',(5.5,8.22167369503577,247.547898263196));
#13637=CARTESIAN_POINT('Origin',(5.5,6.43177298256785,249.937669285906));
#13638=CARTESIAN_POINT('',(-6.5,8.22167369503577,247.547898263196));
#13639=CARTESIAN_POINT('Origin',(-6.5,4.64187227009995,247.547898263196));
#13640=CARTESIAN_POINT('',(5.5,8.22167369503577,247.547898263196));
#13641=CARTESIAN_POINT('Origin',(5.5,6.43177298256785,250.235662713169));
#13642=CARTESIAN_POINT('Origin',(-6.5,4.64187227009995,247.547898263196));
#13643=CARTESIAN_POINT('',(-18.5,4.64187227009995,247.547898263196));
#13644=CARTESIAN_POINT('',(-6.5,4.64187227009995,247.547898263196));
#13645=CARTESIAN_POINT('',(-18.5,8.22167369503577,247.547898263196));
#13646=CARTESIAN_POINT('',(-18.5,8.22167369503577,247.547898263196));
#13647=CARTESIAN_POINT('',(-6.5,8.22167369503577,247.547898263196));
#13648=CARTESIAN_POINT('Origin',(-18.5,6.43177298256785,250.235662713169));
#13649=CARTESIAN_POINT('Origin',(-18.5,6.43177298256785,249.937669285906));
#13650=CARTESIAN_POINT('Origin',(-6.5,6.43177298256785,249.937669285906));
#13651=CARTESIAN_POINT('Origin',(-16.5,16.4317729825679,256.886209595194));
#13652=CARTESIAN_POINT('Origin',(-16.5,16.4317729825679,256.886209595194));
#13653=CARTESIAN_POINT('Origin',(-16.5,-3.56822701743215,256.886209595194));
#13654=CARTESIAN_POINT('Origin',(-16.5,-3.56822701743215,256.886209595194));
#13655=CARTESIAN_POINT('Origin',(3.5,-3.56822701743215,256.886209595194));
#13656=CARTESIAN_POINT('Origin',(3.5,-3.56822701743215,256.886209595194));
#13657=CARTESIAN_POINT('Origin',(3.5,16.4317729825678,256.886209595194));
#13658=CARTESIAN_POINT('Origin',(3.5,16.4317729825678,256.886209595194));
#13659=CARTESIAN_POINT('Origin',(-16.5,-3.56822701743215,256.886209595194));
#13660=CARTESIAN_POINT('',(-18.5,-3.56822701743215,256.886209595194));
#13661=CARTESIAN_POINT('',(-18.5,-3.56822701743215,256.886209595194));
#13662=CARTESIAN_POINT('Origin',(-16.5,-3.56822701743215,256.886209595194));
#13663=CARTESIAN_POINT('Origin',(-18.5,16.4317729825679,256.886209595194));
#13664=CARTESIAN_POINT('',(-18.5,16.4317729825679,256.886209595194));
#13665=CARTESIAN_POINT('',(-18.5,16.4317729825679,256.886209595194));
#13666=CARTESIAN_POINT('',(-18.5,16.4317729825679,256.886209595194));
#13667=CARTESIAN_POINT('Origin',(-16.5,16.4317729825679,256.886209595194));
#13668=CARTESIAN_POINT('',(-16.5,18.4317729825679,256.886209595194));
#13669=CARTESIAN_POINT('',(-16.5,18.4317729825679,256.886209595194));
#13670=CARTESIAN_POINT('Origin',(-16.5,16.4317729825679,256.886209595194));
#13671=CARTESIAN_POINT('Origin',(3.5,18.4317729825679,256.886209595194));
#13672=CARTESIAN_POINT('',(3.5,18.4317729825679,256.886209595194));
#13673=CARTESIAN_POINT('Origin',(-6.5,6.43177298256785,256.886209595194));
#13674=CARTESIAN_POINT('',(0.,0.,0.));
#13675=CARTESIAN_POINT('Origin',(-6.5,6.43177298256785,247.386209595194));
#13676=CARTESIAN_POINT('',(1.5,6.43177298256785,246.886209595194));
#13677=CARTESIAN_POINT('Origin',(-6.5,6.43177298256785,246.886209595194));
#13678=CARTESIAN_POINT('',(0.499999999999999,6.43177298256785,247.886209595194));
#13679=CARTESIAN_POINT('',(0.999999999999999,6.43177298256785,247.386209595194));
#13680=CARTESIAN_POINT('Origin',(-6.5,6.43177298256785,247.886209595194));
#13681=CARTESIAN_POINT('Origin',(-6.5,6.43177298256785,246.886209595194));
#13682=CARTESIAN_POINT('',(0.499999999999999,6.43177298256785,461.946209595194));
#13683=CARTESIAN_POINT('Origin',(-6.5,6.43177298256785,461.946209595194));
#13684=CARTESIAN_POINT('',(0.499999999999999,6.43177298256785,246.886209595194));
#13685=CARTESIAN_POINT('Origin',(-6.5,6.43177298256785,246.886209595194));
#13686=CARTESIAN_POINT('',(2.5,6.43177298256785,246.886209595194));
#13687=CARTESIAN_POINT('Origin',(-6.5,6.43177298256785,246.886209595194));
#13688=CARTESIAN_POINT('Origin',(-6.5,6.43177298256785,462.446209595194));
#13689=CARTESIAN_POINT('',(1.5,6.43177298256785,462.946209595194));
#13690=CARTESIAN_POINT('Origin',(-6.5,6.43177298256785,462.946209595194));
#13691=CARTESIAN_POINT('',(0.999999999999999,6.43177298256785,462.446209595194));
#13692=CARTESIAN_POINT('Origin',(-6.5,6.43177298256785,462.946209595194));
#13693=CARTESIAN_POINT('',(2.5,6.43177298256785,462.946209595194));
#13694=CARTESIAN_POINT('Origin',(-6.5,6.43177298256785,462.946209595194));
#13695=CARTESIAN_POINT('Origin',(-6.5,6.43177298256785,246.886209595194));
#13696=CARTESIAN_POINT('',(2.5,6.43177298256785,246.886209595194));
#13697=CARTESIAN_POINT('',(0.,0.,0.));
#13698=CARTESIAN_POINT('Ctrl Pts',(-12.9,12.1763356291059,464.946209595194));
#13699=CARTESIAN_POINT('Ctrl Pts',(-12.8029959440646,12.3924794841513,464.946209595194));
#13700=CARTESIAN_POINT('Ctrl Pts',(-12.6563710262499,12.683434963611,464.993269980864));
#13701=CARTESIAN_POINT('Ctrl Pts',(-12.5230694771437,12.9192723440419,465.183424929997));
#13702=CARTESIAN_POINT('Ctrl Pts',(-12.5,12.9586405314001,465.291751475466));
#13703=CARTESIAN_POINT('Ctrl Pts',(-12.5,12.9586405314001,465.346209595194));
#13704=CARTESIAN_POINT('Ctrl Pts',(-12.9779309805542,12.2462855353402,464.946209595194));
#13705=CARTESIAN_POINT('Ctrl Pts',(-12.8697226228569,12.4569505293086,464.926883433363));
#13706=CARTESIAN_POINT('Ctrl Pts',(-12.6938330928061,12.7438388264629,464.958568912738));
#13707=CARTESIAN_POINT('Ctrl Pts',(-12.5288182589974,12.9770526459975,465.163348776432));
#13708=CARTESIAN_POINT('Ctrl Pts',(-12.5,13.0160859158435,465.285050299185));
#13709=CARTESIAN_POINT('Ctrl Pts',(-12.5,13.0160859158435,465.346209595194));
#13710=CARTESIAN_POINT('Ctrl Pts',(-13.1330572932533,12.3855250386881,464.859380333003));
#13711=CARTESIAN_POINT('Ctrl Pts',(-12.9815601460676,12.5859161586474,464.824024352416));
#13712=CARTESIAN_POINT('Ctrl Pts',(-12.7386227137214,12.8645013145008,464.854838097387));
#13713=CARTESIAN_POINT('Ctrl Pts',(-12.5140044782818,13.092657901597,465.113239520754));
#13714=CARTESIAN_POINT('Ctrl Pts',(-12.4748408805091,13.1309318538629,465.268197789592));
#13715=CARTESIAN_POINT('Ctrl Pts',(-12.4748408805091,13.1309318538629,465.346209595194));
#13716=CARTESIAN_POINT('Ctrl Pts',(-13.1976744186047,12.44352458941,464.650929350314));
#13717=CARTESIAN_POINT('Ctrl Pts',(-13.0056838626847,12.6568334505882,464.638779692075));
#13718=CARTESIAN_POINT('Ctrl Pts',(-12.7145954604713,12.9482471139396,464.711880095389));
#13719=CARTESIAN_POINT('Ctrl Pts',(-12.4497756270675,13.1850735534976,465.051466709479));
#13720=CARTESIAN_POINT('Ctrl Pts',(-12.4040626064597,13.2248094693827,465.247599949711));
#13721=CARTESIAN_POINT('Ctrl Pts',(-12.4040626064597,13.2248094693827,465.346209595194));
#13722=CARTESIAN_POINT('Ctrl Pts',(-13.1976744186047,12.44352458941,464.546209595194));
#13723=CARTESIAN_POINT('Ctrl Pts',(-12.9946426736236,12.6697216470157,464.546209595194));
#13724=CARTESIAN_POINT('Ctrl Pts',(-12.6877533107556,12.9742099394735,464.640330366534));
#13725=CARTESIAN_POINT('Ctrl Pts',(-12.4087500684403,13.2210165003895,465.020640264799));
#13726=CARTESIAN_POINT('Ctrl Pts',(-12.3604651162791,13.2622157662295,465.237293355737));
#13727=CARTESIAN_POINT('Ctrl Pts',(-12.3604651162791,13.2622157662295,465.346209595194));
#13728=CARTESIAN_POINT('',(-12.5,12.9586405314001,465.346209595194));
#13729=CARTESIAN_POINT('',(-12.9,12.1763356291059,464.946209595194));
#13730=CARTESIAN_POINT('Ctrl Pts',(-12.9,12.1763356291059,464.946209595194));
#13731=CARTESIAN_POINT('Ctrl Pts',(-12.8029959440646,12.3924794841513,464.946209595194));
#13732=CARTESIAN_POINT('Ctrl Pts',(-12.6563710262499,12.683434963611,464.993269980864));
#13733=CARTESIAN_POINT('Ctrl Pts',(-12.5230694771437,12.9192723440419,465.183424929997));
#13734=CARTESIAN_POINT('Ctrl Pts',(-12.5,12.9586405314001,465.291751475466));
#13735=CARTESIAN_POINT('Ctrl Pts',(-12.5,12.9586405314001,465.346209595194));
#13736=CARTESIAN_POINT('',(-12.3604651162791,13.2622157662296,465.346209595194));
#13737=CARTESIAN_POINT('Origin',(-12.1,12.9586405314001,465.346209595194));
#13738=CARTESIAN_POINT('',(-13.1976744186047,12.44352458941,464.546209595194));
#13739=CARTESIAN_POINT('Ctrl Pts',(-12.3604651162791,13.2622157662295,465.346209595194));
#13740=CARTESIAN_POINT('Ctrl Pts',(-12.3604651162791,13.2622157662295,465.237293355737));
#13741=CARTESIAN_POINT('Ctrl Pts',(-12.4087500684403,13.2210165003895,465.020640264799));
#13742=CARTESIAN_POINT('Ctrl Pts',(-12.6877533107556,12.9742099394735,464.640330366534));
#13743=CARTESIAN_POINT('Ctrl Pts',(-12.9946426736236,12.6697216470157,464.546209595194));
#13744=CARTESIAN_POINT('Ctrl Pts',(-13.1976744186047,12.44352458941,464.546209595194));
#13745=CARTESIAN_POINT('Origin',(-12.9,12.1763356291059,464.546209595194));
#13746=CARTESIAN_POINT('Ctrl Pts',(-12.5,-0.0950945662644365,465.346209595194));
#13747=CARTESIAN_POINT('Ctrl Pts',(-12.5,-0.0950945662644367,465.29175196324));
#13748=CARTESIAN_POINT('Ctrl Pts',(-12.5230712817632,-0.055723237524717,
465.183423780398));
#13749=CARTESIAN_POINT('Ctrl Pts',(-12.6563723650316,0.180113321251888,
464.993272151286));
#13750=CARTESIAN_POINT('Ctrl Pts',(-12.8029968129178,0.471068416957768,
464.946209595194));
#13751=CARTESIAN_POINT('Ctrl Pts',(-12.9,0.687210336029828,464.946209595194));
#13752=CARTESIAN_POINT('Ctrl Pts',(-12.5,-0.152539950707804,465.346209595194));
#13753=CARTESIAN_POINT('Ctrl Pts',(-12.5,-0.152539950707804,465.285050846981));
#13754=CARTESIAN_POINT('Ctrl Pts',(-12.5288205011401,-0.113503572746219,
465.163347579182));
#13755=CARTESIAN_POINT('Ctrl Pts',(-12.6938347824102,0.119709443021527,
464.958571481921));
#13756=CARTESIAN_POINT('Ctrl Pts',(-12.8697235920656,0.406597322726993,
464.926883606465));
#13757=CARTESIAN_POINT('Ctrl Pts',(-12.9779309805542,0.617260429795526,
464.946209595194));
#13758=CARTESIAN_POINT('Ctrl Pts',(-12.4748409267651,-0.267385909988173,
465.346209595194));
#13759=CARTESIAN_POINT('Ctrl Pts',(-12.4748409267651,-0.267385909988173,
465.268198488334));
#13760=CARTESIAN_POINT('Ctrl Pts',(-12.5140076158955,-0.229108956409242,
465.113238091813));
#13761=CARTESIAN_POINT('Ctrl Pts',(-12.7386250832635,-0.000953121784120126,
464.854841435699));
#13762=CARTESIAN_POINT('Ctrl Pts',(-12.9815617779372,0.277631354593801,
464.82402503853));
#13763=CARTESIAN_POINT('Ctrl Pts',(-13.1330575681819,0.478020679674991,
464.859380702438));
#13764=CARTESIAN_POINT('Ctrl Pts',(-12.4040626064597,-0.361263504247002,
465.346209595194));
#13765=CARTESIAN_POINT('Ctrl Pts',(-12.4040626064597,-0.361263504247002,
465.247600832946));
#13766=CARTESIAN_POINT('Ctrl Pts',(-12.4497792119805,-0.32152443178383,
465.051464677961));
#13767=CARTESIAN_POINT('Ctrl Pts',(-12.7145981275216,-0.0846988078642869,
464.711884088098));
#13768=CARTESIAN_POINT('Ctrl Pts',(-13.00568558232,0.206714425128216,464.638779800898));
#13769=CARTESIAN_POINT('Ctrl Pts',(-13.1976744186047,0.42002137572574,464.650929350314));
#13770=CARTESIAN_POINT('Ctrl Pts',(-12.3604651162791,-0.398669801093845,
465.346209595194));
#13771=CARTESIAN_POINT('Ctrl Pts',(-12.3604651162791,-0.398669801093846,
465.237294331286));
#13772=CARTESIAN_POINT('Ctrl Pts',(-12.4087538455509,-0.357467247761575,
465.020637965603));
#13773=CARTESIAN_POINT('Ctrl Pts',(-12.6877561128567,-0.110661546716286,
464.640334707378));
#13774=CARTESIAN_POINT('Ctrl Pts',(-12.9946444921535,0.1938263441387,464.546209595194));
#13775=CARTESIAN_POINT('Ctrl Pts',(-13.1976744186047,0.42002137572574,464.546209595194));
#13776=CARTESIAN_POINT('',(-13.1976744186047,0.420021375725734,464.546209595194));
#13777=CARTESIAN_POINT('',(-12.3604651162791,-0.398669801093845,465.346209595194));
#13778=CARTESIAN_POINT('Ctrl Pts',(-13.1976744186047,0.42002137572574,464.546209595194));
#13779=CARTESIAN_POINT('Ctrl Pts',(-12.9946444921535,0.1938263441387,464.546209595194));
#13780=CARTESIAN_POINT('Ctrl Pts',(-12.6877561128567,-0.110661546716286,
464.640334707378));
#13781=CARTESIAN_POINT('Ctrl Pts',(-12.4087538455509,-0.357467247761575,
465.020637965603));
#13782=CARTESIAN_POINT('Ctrl Pts',(-12.3604651162791,-0.398669801093846,
465.237294331286));
#13783=CARTESIAN_POINT('Ctrl Pts',(-12.3604651162791,-0.398669801093845,
465.346209595194));
#13784=CARTESIAN_POINT('',(-12.5,-0.0950945662644354,465.346209595194));
#13785=CARTESIAN_POINT('Origin',(-12.1,-0.0950945662644354,465.346209595194));
#13786=CARTESIAN_POINT('',(-12.9,0.687210336029827,464.946209595194));
#13787=CARTESIAN_POINT('Ctrl Pts',(-12.5,-0.0950945662644365,465.346209595194));
#13788=CARTESIAN_POINT('Ctrl Pts',(-12.5,-0.0950945662644367,465.29175196324));
#13789=CARTESIAN_POINT('Ctrl Pts',(-12.5230712817632,-0.055723237524717,
465.183423780398));
#13790=CARTESIAN_POINT('Ctrl Pts',(-12.6563723650316,0.180113321251888,
464.993272151286));
#13791=CARTESIAN_POINT('Ctrl Pts',(-12.8029968129178,0.471068416957768,
464.946209595194));
#13792=CARTESIAN_POINT('Ctrl Pts',(-12.9,0.687210336029828,464.946209595194));
#13793=CARTESIAN_POINT('Origin',(-12.9,0.687210336029829,464.546209595194));
#13794=CARTESIAN_POINT('Origin',(-12.1,12.9586405314001,462.946209595194));
#13795=CARTESIAN_POINT('',(-12.5,12.9586405314001,476.446209595194));
#13796=CARTESIAN_POINT('',(-12.3604651162791,13.2622157662296,476.446209595194));
#13797=CARTESIAN_POINT('Origin',(-12.1,12.9586405314001,476.446209595194));
#13798=CARTESIAN_POINT('',(-12.3604651162791,13.2622157662296,462.946209595194));
#13799=CARTESIAN_POINT('',(-12.5,12.9586405314001,462.946209595194));
#13800=CARTESIAN_POINT('Ctrl Pts',(-12.5,12.9586405314001,476.446209595194));
#13801=CARTESIAN_POINT('Ctrl Pts',(-12.5,12.9586405314002,476.853861255764));
#13802=CARTESIAN_POINT('Ctrl Pts',(-12.5,12.7121305874131,477.448240925556));
#13803=CARTESIAN_POINT('Ctrl Pts',(-12.5,11.6095151659742,478.389250767395));
#13804=CARTESIAN_POINT('Ctrl Pts',(-12.5,10.5470763037083,478.546209595194));
#13805=CARTESIAN_POINT('Ctrl Pts',(-12.5,9.73177298256796,478.546209595194));
#13806=CARTESIAN_POINT('Ctrl Pts',(-12.5,13.0160859158435,476.446209595194));
#13807=CARTESIAN_POINT('Ctrl Pts',(-12.5,13.0160859158436,476.868556690467));
#13808=CARTESIAN_POINT('Ctrl Pts',(-12.499798919425,12.7644563196739,477.484521897399));
#13809=CARTESIAN_POINT('Ctrl Pts',(-12.4999487018801,11.6399911364717,478.465534436156));
#13810=CARTESIAN_POINT('Ctrl Pts',(-12.4996309047003,10.5575748644185,478.639497203128));
#13811=CARTESIAN_POINT('Ctrl Pts',(-12.5,9.73177298256796,478.650929350314));
#13812=CARTESIAN_POINT('Ctrl Pts',(-12.4748408382406,13.1309318344346,476.446209595194));
#13813=CARTESIAN_POINT('Ctrl Pts',(-12.4748408382406,13.1309318344347,476.897925676163));
#13814=CARTESIAN_POINT('Ctrl Pts',(-12.4714917573037,12.8690363604298,477.557273431096));
#13815=CARTESIAN_POINT('Ctrl Pts',(-12.4543886115941,11.7008031686518,478.618026795867));
#13816=CARTESIAN_POINT('Ctrl Pts',(-12.4330371840754,10.5783878700328,478.826112000052));
#13817=CARTESIAN_POINT('Ctrl Pts',(-12.4131704002205,9.73177298256796,478.859379995414));
#13818=CARTESIAN_POINT('Ctrl Pts',(-12.4040626064597,13.2248094693827,476.446209595194));
#13819=CARTESIAN_POINT('Ctrl Pts',(-12.4040626064597,13.2248094693828,476.921954463457));
#13820=CARTESIAN_POINT('Ctrl Pts',(-12.3915856347517,12.9517896616252,477.615790277435));
#13821=CARTESIAN_POINT('Ctrl Pts',(-12.3316250640951,11.7391724081509,478.725157762151));
#13822=CARTESIAN_POINT('Ctrl Pts',(-12.2613563482675,10.587188239976,478.928024760507));
#13823=CARTESIAN_POINT('Ctrl Pts',(-12.2047197551197,9.73177298256796,478.946209595194));
#13824=CARTESIAN_POINT('Ctrl Pts',(-12.3604651162791,13.2622157662295,476.446209595194));
#13825=CARTESIAN_POINT('Ctrl Pts',(-12.3604651162791,13.2622157662296,476.931509191111));
#13826=CARTESIAN_POINT('Ctrl Pts',(-12.342893213559,12.9832980857263,477.639104036101));
#13827=CARTESIAN_POINT('Ctrl Pts',(-12.2600218813812,11.7488052197396,478.759353847815));
#13828=CARTESIAN_POINT('Ctrl Pts',(-12.167925862495,10.5871040441072,478.946209595194));
#13829=CARTESIAN_POINT('Ctrl Pts',(-12.1,9.73177298256796,478.946209595194));
#13830=CARTESIAN_POINT('',(-12.5,9.73177298256795,478.546209595194));
#13831=CARTESIAN_POINT('',(-12.1,9.73177298256795,478.946209595194));
#13832=CARTESIAN_POINT('Origin',(-12.1,9.73177298256795,478.546209595194));
#13833=CARTESIAN_POINT('Ctrl Pts',(-12.1,9.73177298256796,478.946209595194));
#13834=CARTESIAN_POINT('Ctrl Pts',(-12.167925862495,10.5871040441072,478.946209595194));
#13835=CARTESIAN_POINT('Ctrl Pts',(-12.2600218813812,11.7488052197396,478.759353847815));
#13836=CARTESIAN_POINT('Ctrl Pts',(-12.342893213559,12.9832980857263,477.639104036101));
#13837=CARTESIAN_POINT('Ctrl Pts',(-12.3604651162791,13.2622157662296,476.931509191111));
#13838=CARTESIAN_POINT('Ctrl Pts',(-12.3604651162791,13.2622157662295,476.446209595194));
#13839=CARTESIAN_POINT('Ctrl Pts',(-12.5,12.9586405314001,476.446209595194));
#13840=CARTESIAN_POINT('Ctrl Pts',(-12.5,12.9586405314002,476.853861255764));
#13841=CARTESIAN_POINT('Ctrl Pts',(-12.5,12.7121305874131,477.448240925556));
#13842=CARTESIAN_POINT('Ctrl Pts',(-12.5,11.6095151659742,478.389250767395));
#13843=CARTESIAN_POINT('Ctrl Pts',(-12.5,10.5470763037083,478.546209595194));
#13844=CARTESIAN_POINT('Ctrl Pts',(-12.5,9.73177298256796,478.546209595194));
#13845=CARTESIAN_POINT('Origin',(-12.1,9.78587494881754,478.546209595194));
#13846=CARTESIAN_POINT('',(-12.5,3.13177298256785,478.546209595194));
#13847=CARTESIAN_POINT('',(-12.1,3.13177298256785,478.946209595194));
#13848=CARTESIAN_POINT('Origin',(-12.1,3.13177298256785,478.546209595194));
#13849=CARTESIAN_POINT('',(-12.1,9.78587494881754,478.946209595194));
#13850=CARTESIAN_POINT('',(-12.5,9.78587494881754,478.546209595194));
#13851=CARTESIAN_POINT('Ctrl Pts',(-12.5,3.13177298256785,478.546209595194));
#13852=CARTESIAN_POINT('Ctrl Pts',(-12.5,2.52026774111634,478.546209595194));
#13853=CARTESIAN_POINT('Ctrl Pts',(-12.5,1.48936227736903,478.433754771008));
#13854=CARTESIAN_POINT('Ctrl Pts',(-12.5,0.244282023002687,477.649528864133));
#13855=CARTESIAN_POINT('Ctrl Pts',(-12.5,-0.0950945662644376,476.853879756162));
#13856=CARTESIAN_POINT('Ctrl Pts',(-12.5,-0.0950945662644376,476.446209595194));
#13857=CARTESIAN_POINT('Ctrl Pts',(-12.5,3.13177298256785,478.650929350314));
#13858=CARTESIAN_POINT('Ctrl Pts',(-12.4997231659623,2.51239346324273,478.642354850807));
#13859=CARTESIAN_POINT('Ctrl Pts',(-12.4998708957056,1.46352149007596,478.513649678176));
#13860=CARTESIAN_POINT('Ctrl Pts',(-12.4997435365771,0.193842442444793,
477.69306379392));
#13861=CARTESIAN_POINT('Ctrl Pts',(-12.5,-0.152539950707804,476.868575857786));
#13862=CARTESIAN_POINT('Ctrl Pts',(-12.5,-0.152539950707804,476.446209595194));
#13863=CARTESIAN_POINT('Ctrl Pts',(-12.4131706406899,3.13177298256785,478.859380235884));
#13864=CARTESIAN_POINT('Ctrl Pts',(-12.4280714047896,2.49678300061667,478.834428107014));
#13865=CARTESIAN_POINT('Ctrl Pts',(-12.4502945445776,1.41200273935032,478.673426816548));
#13866=CARTESIAN_POINT('Ctrl Pts',(-12.4703420994035,0.0930418380396119,
477.780378953069));
#13867=CARTESIAN_POINT('Ctrl Pts',(-12.4748408683491,-0.267385883137938,
476.89794617633));
#13868=CARTESIAN_POINT('Ctrl Pts',(-12.4748408683491,-0.267385883137938,
476.446209595194));
#13869=CARTESIAN_POINT('Ctrl Pts',(-12.2047197551197,3.13177298256785,478.946209595194));
#13870=CARTESIAN_POINT('Ctrl Pts',(-12.2471991277284,2.49018242361983,478.932570350219));
#13871=CARTESIAN_POINT('Ctrl Pts',(-12.3174618184511,1.38194921130776,478.780697709241));
#13872=CARTESIAN_POINT('Ctrl Pts',(-12.387272273891,0.014706061216163,477.850660975865));
#13873=CARTESIAN_POINT('Ctrl Pts',(-12.4040626064597,-0.361263504247001,
476.921976054119));
#13874=CARTESIAN_POINT('Ctrl Pts',(-12.4040626064597,-0.361263504247001,
476.446209595194));
#13875=CARTESIAN_POINT('Ctrl Pts',(-12.1,3.13177298256785,478.946209595194));
#13876=CARTESIAN_POINT('Ctrl Pts',(-12.1509467088736,2.49024557338726,478.946209595194));
#13877=CARTESIAN_POINT('Ctrl Pts',(-12.2408287043769,1.37587602390371,478.812334804496));
#13878=CARTESIAN_POINT('Ctrl Pts',(-12.3367447800671,-0.0143093659240391,
477.878732534407));
#13879=CARTESIAN_POINT('Ctrl Pts',(-12.3604651162791,-0.398669801093845,
476.931531215393));
#13880=CARTESIAN_POINT('Ctrl Pts',(-12.3604651162791,-0.398669801093845,
476.446209595194));
#13881=CARTESIAN_POINT('',(-12.5,-0.0950945662644376,476.446209595194));
#13882=CARTESIAN_POINT('',(-12.3604651162791,-0.398669801093845,476.446209595194));
#13883=CARTESIAN_POINT('Origin',(-12.1,-0.0950945662644365,476.446209595194));
#13884=CARTESIAN_POINT('Ctrl Pts',(-12.3604651162791,-0.398669801093845,
476.446209595194));
#13885=CARTESIAN_POINT('Ctrl Pts',(-12.3604651162791,-0.398669801093845,
476.931531215393));
#13886=CARTESIAN_POINT('Ctrl Pts',(-12.3367447800671,-0.0143093659240391,
477.878732534407));
#13887=CARTESIAN_POINT('Ctrl Pts',(-12.2408287043769,1.37587602390371,478.812334804496));
#13888=CARTESIAN_POINT('Ctrl Pts',(-12.1509467088736,2.49024557338726,478.946209595194));
#13889=CARTESIAN_POINT('Ctrl Pts',(-12.1,3.13177298256785,478.946209595194));
#13890=CARTESIAN_POINT('Ctrl Pts',(-12.5,3.13177298256785,478.546209595194));
#13891=CARTESIAN_POINT('Ctrl Pts',(-12.5,2.52026774111634,478.546209595194));
#13892=CARTESIAN_POINT('Ctrl Pts',(-12.5,1.48936227736903,478.433754771008));
#13893=CARTESIAN_POINT('Ctrl Pts',(-12.5,0.244282023002687,477.649528864133));
#13894=CARTESIAN_POINT('Ctrl Pts',(-12.5,-0.0950945662644376,476.853879756162));
#13895=CARTESIAN_POINT('Ctrl Pts',(-12.5,-0.0950945662644376,476.446209595194));
#13896=CARTESIAN_POINT('Origin',(-12.1,-0.0950945662644354,462.946209595194));
#13897=CARTESIAN_POINT('',(-12.3604651162791,-0.398669801093845,462.946209595194));
#13898=CARTESIAN_POINT('',(-12.5,-0.0950945662644354,462.946209595194));
#13899=CARTESIAN_POINT('Origin',(-12.9,9.78587494881754,465.346209595194));
#13900=CARTESIAN_POINT('',(-12.5,9.78587494881754,465.346209595194));
#13901=CARTESIAN_POINT('',(-12.9,9.78587494881754,464.946209595194));
#13902=CARTESIAN_POINT('Origin',(-6.5,6.43177298256785,464.546209595194));
#13903=CARTESIAN_POINT('',(-15.5,6.43177298256785,464.546209595194));
#13904=CARTESIAN_POINT('Origin',(-6.5,6.43177298256785,464.546209595194));
#13905=CARTESIAN_POINT('Origin',(-6.5,6.43177298256785,464.546209595194));
#13906=CARTESIAN_POINT('Origin',(-6.5,6.43177298256785,464.946209595194));
#13907=CARTESIAN_POINT('Origin',(-6.5,6.43177298256785,478.946209595194));
#13908=CARTESIAN_POINT('',(-0.900000000000017,3.13177298256776,478.946209595194));
#13909=CARTESIAN_POINT('Origin',(-6.5,6.43177298256785,478.946209595194));
#13910=CARTESIAN_POINT('',(-0.899999999999997,9.73177298256785,478.946209595194));
#13911=CARTESIAN_POINT('',(-0.899999999999997,3.07767101631817,478.946209595194));
#13912=CARTESIAN_POINT('Origin',(-6.5,6.43177298256785,478.946209595194));
#13913=CARTESIAN_POINT('Origin',(-6.5,6.43177298256785,476.446209595194));
#13914=CARTESIAN_POINT('',(-0.639534883720928,-0.398669801093843,476.446209595194));
#13915=CARTESIAN_POINT('Origin',(-6.5,6.43177298256785,476.446209595194));
#13916=CARTESIAN_POINT('Ctrl Pts',(-0.899999999999989,3.13177298256775,
478.946209595194));
#13917=CARTESIAN_POINT('Ctrl Pts',(-0.83207413779171,2.27644192463902,478.946209595194));
#13918=CARTESIAN_POINT('Ctrl Pts',(-0.739978110974983,1.11474130806174,
478.759354402431));
#13919=CARTESIAN_POINT('Ctrl Pts',(-0.657106776481008,-0.119751885582937,
477.639104541356));
#13920=CARTESIAN_POINT('Ctrl Pts',(-0.639534883720916,-0.398669801093799,
476.93150918906));
#13921=CARTESIAN_POINT('Ctrl Pts',(-0.639534883720934,-0.398669801093842,
476.446209595194));
#13922=CARTESIAN_POINT('Origin',(-12.5,13.1399769150672,478.946209595194));
#13923=CARTESIAN_POINT('',(-12.5,10.4317729825678,471.090577685893));
#13924=CARTESIAN_POINT('Origin',(-12.5,6.43177298256785,471.090577685893));
#13925=CARTESIAN_POINT('Origin',(-14.,6.43177298256785,464.946209595194));
#13926=CARTESIAN_POINT('Ctrl Pts',(-0.499999999999996,12.9586405314001,
465.346209595194));
#13927=CARTESIAN_POINT('Ctrl Pts',(-0.499999999999997,12.9586405314001,
465.291751963028));
#13928=CARTESIAN_POINT('Ctrl Pts',(-0.476928716540935,12.9192691993652,
465.183423779369));
#13929=CARTESIAN_POINT('Ctrl Pts',(-0.34362763610145,12.6834326448933,464.993272154916));
#13930=CARTESIAN_POINT('Ctrl Pts',(-0.197003187459576,12.3924775490188,
464.946209595194));
#13931=CARTESIAN_POINT('Ctrl Pts',(-0.0999999999999975,12.1763356291059,
464.946209595194));
#13932=CARTESIAN_POINT('Ctrl Pts',(-0.499999999999996,13.0160859158435,
465.346209595194));
#13933=CARTESIAN_POINT('Ctrl Pts',(-0.499999999999997,13.0160859158435,
465.285050846744));
#13934=CARTESIAN_POINT('Ctrl Pts',(-0.471179496785347,12.9770495346129,
465.16334757817));
#13935=CARTESIAN_POINT('Ctrl Pts',(-0.306165219154938,12.7438365231285,
464.958571486081));
#13936=CARTESIAN_POINT('Ctrl Pts',(-0.130276408355345,12.4569486432282,
464.92688360639));
#13937=CARTESIAN_POINT('Ctrl Pts',(-0.0220690194458337,12.2462855353402,
464.946209595194));
#13938=CARTESIAN_POINT('Ctrl Pts',(-0.525159075955398,13.1309318738734,
465.346209595194));
#13939=CARTESIAN_POINT('Ctrl Pts',(-0.525159075955398,13.1309318738734,
465.26819848803));
#13940=CARTESIAN_POINT('Ctrl Pts',(-0.4859923865512,13.0926549146057,465.113238086588));
#13941=CARTESIAN_POINT('Ctrl Pts',(-0.261374923085867,12.8644990852749,
464.85484143889));
#13942=CARTESIAN_POINT('Ctrl Pts',(-0.0184382388215931,12.585914596808,
464.824025016665));
#13943=CARTESIAN_POINT('Ctrl Pts',(0.133057552012535,12.3855252709472,464.859380680711));
#13944=CARTESIAN_POINT('Ctrl Pts',(-0.595937393540275,13.2248094693827,
465.346209595194));
#13945=CARTESIAN_POINT('Ctrl Pts',(-0.595937393540275,13.2248094693827,
465.247600832562));
#13946=CARTESIAN_POINT('Ctrl Pts',(-0.550220784700754,13.1850703935657,
465.051464676199));
#13947=CARTESIAN_POINT('Ctrl Pts',(-0.285401874822712,12.9482447739809,
464.711884094779));
#13948=CARTESIAN_POINT('Ctrl Pts',(0.00568558157314103,12.6568315408373,
464.63877980085));
#13949=CARTESIAN_POINT('Ctrl Pts',(0.197674418604646,12.44352458941,464.650929350314));
#13950=CARTESIAN_POINT('Ctrl Pts',(-0.639534883720927,13.2622157662295,
465.346209595194));
#13951=CARTESIAN_POINT('Ctrl Pts',(-0.639534883720927,13.2622157662295,
465.237294330863));
#13952=CARTESIAN_POINT('Ctrl Pts',(-0.591246150899638,13.2210132094488,
465.020637963544));
#13953=CARTESIAN_POINT('Ctrl Pts',(-0.31224388951466,12.9742075129084,464.640334714638));
#13954=CARTESIAN_POINT('Ctrl Pts',(-0.00535550863633265,12.6697196218769,
464.546209595194));
#13955=CARTESIAN_POINT('Ctrl Pts',(0.197674418604645,12.44352458941,464.546209595194));
#13956=CARTESIAN_POINT('',(0.197674418604654,12.44352458941,464.546209595194));
#13957=CARTESIAN_POINT('',(-0.639534883720926,13.2622157662295,465.346209595194));
#13958=CARTESIAN_POINT('Ctrl Pts',(0.197674418604645,12.44352458941,464.546209595194));
#13959=CARTESIAN_POINT('Ctrl Pts',(-0.00535550863633265,12.6697196218769,
464.546209595194));
#13960=CARTESIAN_POINT('Ctrl Pts',(-0.31224388951466,12.9742075129084,464.640334714638));
#13961=CARTESIAN_POINT('Ctrl Pts',(-0.591246150899638,13.2210132094488,
465.020637963544));
#13962=CARTESIAN_POINT('Ctrl Pts',(-0.639534883720927,13.2622157662295,
465.237294330863));
#13963=CARTESIAN_POINT('Ctrl Pts',(-0.639534883720927,13.2622157662295,
465.346209595194));
#13964=CARTESIAN_POINT('',(-0.499999999999997,12.9586405314001,465.346209595194));
#13965=CARTESIAN_POINT('Origin',(-0.899999999999996,12.9586405314001,465.346209595194));
#13966=CARTESIAN_POINT('',(-0.0999999999999979,12.1763356291059,464.946209595194));
#13967=CARTESIAN_POINT('Ctrl Pts',(-0.499999999999996,12.9586405314001,
465.346209595194));
#13968=CARTESIAN_POINT('Ctrl Pts',(-0.499999999999997,12.9586405314001,
465.291751963028));
#13969=CARTESIAN_POINT('Ctrl Pts',(-0.476928716540935,12.9192691993652,
465.183423779369));
#13970=CARTESIAN_POINT('Ctrl Pts',(-0.34362763610145,12.6834326448933,464.993272154916));
#13971=CARTESIAN_POINT('Ctrl Pts',(-0.197003187459576,12.3924775490188,
464.946209595194));
#13972=CARTESIAN_POINT('Ctrl Pts',(-0.0999999999999975,12.1763356291059,
464.946209595194));
#13973=CARTESIAN_POINT('Origin',(-0.0999999999999979,12.1763356291059,464.546209595194));
#13974=CARTESIAN_POINT('Ctrl Pts',(-0.0999999999999936,0.687210336029823,
464.946209595194));
#13975=CARTESIAN_POINT('Ctrl Pts',(-0.197004053805406,0.471066485730349,
464.946209595194));
#13976=CARTESIAN_POINT('Ctrl Pts',(-0.343628961915439,0.180111016895773,
464.993269988545));
#13977=CARTESIAN_POINT('Ctrl Pts',(-0.476930512726993,-0.0557263627151083,
465.183424919342));
#13978=CARTESIAN_POINT('Ctrl Pts',(-0.499999999999998,-0.0950945662644381,
465.291751476661));
#13979=CARTESIAN_POINT('Ctrl Pts',(-0.499999999999998,-0.0950945662644381,
465.346209595194));
#13980=CARTESIAN_POINT('Ctrl Pts',(-0.0220690194458293,0.617260429795521,
464.946209595194));
#13981=CARTESIAN_POINT('Ctrl Pts',(-0.130277374767095,0.406595440452743,
464.926883433788));
#13982=CARTESIAN_POINT('Ctrl Pts',(-0.306166894624085,0.119707152456133,
464.95856892495));
#13983=CARTESIAN_POINT('Ctrl Pts',(-0.471181729397159,-0.113506665586292,
465.16334876686));
#13984=CARTESIAN_POINT('Ctrl Pts',(-0.499999999999998,-0.152539950707803,
465.285050300528));
#13985=CARTESIAN_POINT('Ctrl Pts',(-0.499999999999998,-0.152539950707804,
465.346209595194));
#13986=CARTESIAN_POINT('Ctrl Pts',(0.133057850423733,0.47802042633817,464.859381081701));
#13987=CARTESIAN_POINT('Ctrl Pts',(-0.0184392934354909,0.277629310778949,
464.82402510189));
#13988=CARTESIAN_POINT('Ctrl Pts',(-0.261377121062116,-0.000955430391377806,
464.854838190806));
#13989=CARTESIAN_POINT('Ctrl Pts',(-0.485995323452632,-0.229112051155817,
465.113239647082));
#13990=CARTESIAN_POINT('Ctrl Pts',(-0.525159025748574,-0.267385931814736,
465.268197791304));
#13991=CARTESIAN_POINT('Ctrl Pts',(-0.525159025748574,-0.267385931814736,
465.346209595194));
#13992=CARTESIAN_POINT('Ctrl Pts',(0.197674418604656,0.420021375725734,
464.650929350314));
#13993=CARTESIAN_POINT('Ctrl Pts',(0.00568386690033115,0.206712519231232,
464.638779692341));
#13994=CARTESIAN_POINT('Ctrl Pts',(-0.28540451322635,-0.0847011369192216,
464.711880110167));
#13995=CARTESIAN_POINT('Ctrl Pts',(-0.550224351095307,-0.32152757410988,
465.051466690852));
#13996=CARTESIAN_POINT('Ctrl Pts',(-0.595937393540273,-0.361263504246996,
465.247599951876));
#13997=CARTESIAN_POINT('Ctrl Pts',(-0.595937393540273,-0.361263504246996,
465.346209595194));
#13998=CARTESIAN_POINT('Ctrl Pts',(0.197674418604656,0.420021375725734,
464.546209595194));
#13999=CARTESIAN_POINT('Ctrl Pts',(-0.0053573219182965,0.193824323086751,
464.546209595194));
#14000=CARTESIAN_POINT('Ctrl Pts',(-0.31224666447418,-0.110663958251744,
464.640330381896));
#14001=CARTESIAN_POINT('Ctrl Pts',(-0.591249910358824,-0.357470518309637,
465.020640243491));
#14002=CARTESIAN_POINT('Ctrl Pts',(-0.639534883720924,-0.398669801093839,
465.237293358129));
#14003=CARTESIAN_POINT('Ctrl Pts',(-0.639534883720924,-0.398669801093839,
465.346209595194));
#14004=CARTESIAN_POINT('',(-0.499999999999998,-0.0950945662644331,465.346209595194));
#14005=CARTESIAN_POINT('',(-0.0999999999999979,0.687210336029828,464.946209595194));
#14006=CARTESIAN_POINT('Ctrl Pts',(-0.0999999999999936,0.687210336029823,
464.946209595194));
#14007=CARTESIAN_POINT('Ctrl Pts',(-0.197004053805406,0.471066485730349,
464.946209595194));
#14008=CARTESIAN_POINT('Ctrl Pts',(-0.343628961915439,0.180111016895773,
464.993269988545));
#14009=CARTESIAN_POINT('Ctrl Pts',(-0.476930512726993,-0.0557263627151083,
465.183424919342));
#14010=CARTESIAN_POINT('Ctrl Pts',(-0.499999999999998,-0.0950945662644381,
465.291751476661));
#14011=CARTESIAN_POINT('Ctrl Pts',(-0.499999999999998,-0.0950945662644381,
465.346209595194));
#14012=CARTESIAN_POINT('',(-0.639534883720928,-0.398669801093843,465.346209595194));
#14013=CARTESIAN_POINT('Origin',(-0.899999999999999,-0.0950945662644331,
465.346209595194));
#14014=CARTESIAN_POINT('',(0.197674418604655,0.420021375725734,464.546209595194));
#14015=CARTESIAN_POINT('Ctrl Pts',(-0.639534883720924,-0.398669801093839,
465.346209595194));
#14016=CARTESIAN_POINT('Ctrl Pts',(-0.639534883720924,-0.398669801093839,
465.237293358129));
#14017=CARTESIAN_POINT('Ctrl Pts',(-0.591249910358824,-0.357470518309637,
465.020640243491));
#14018=CARTESIAN_POINT('Ctrl Pts',(-0.31224666447418,-0.110663958251744,
464.640330381896));
#14019=CARTESIAN_POINT('Ctrl Pts',(-0.0053573219182965,0.193824323086751,
464.546209595194));
#14020=CARTESIAN_POINT('Ctrl Pts',(0.197674418604656,0.420021375725734,
464.546209595194));
#14021=CARTESIAN_POINT('Origin',(-0.0999999999999979,0.687210336029827,
464.546209595194));
#14022=CARTESIAN_POINT('Origin',(-0.899999999999999,-0.0950945662644331,
462.946209595194));
#14023=CARTESIAN_POINT('',(-0.499999999999998,-0.0950945662644331,476.446209595194));
#14024=CARTESIAN_POINT('Origin',(-0.899999999999999,-0.0950945662644331,
476.446209595194));
#14025=CARTESIAN_POINT('',(-0.639534883720928,-0.398669801093843,462.946209595194));
#14026=CARTESIAN_POINT('',(-0.499999999999998,-0.0950945662644331,462.946209595194));
#14027=CARTESIAN_POINT('Ctrl Pts',(-0.499999999999998,-0.0950945662644388,
476.446209595194));
#14028=CARTESIAN_POINT('Ctrl Pts',(-0.499999999999998,-0.0950945662643835,
476.853861254042));
#14029=CARTESIAN_POINT('Ctrl Pts',(-0.499999999999998,0.151415578718571,
477.44824134997));
#14030=CARTESIAN_POINT('Ctrl Pts',(-0.499999999999998,1.25403127909223,
478.389251233274));
#14031=CARTESIAN_POINT('Ctrl Pts',(-0.499999999999998,2.31646966486893,
478.546209595194));
#14032=CARTESIAN_POINT('Ctrl Pts',(-0.499999999999998,3.13177298256775,
478.546209595194));
#14033=CARTESIAN_POINT('Ctrl Pts',(-0.5,-0.152539950707805,476.446209595194));
#14034=CARTESIAN_POINT('Ctrl Pts',(-0.499999999999997,-0.152539950707749,
476.868556688683));
#14035=CARTESIAN_POINT('Ctrl Pts',(-0.500201055627566,0.0990898464205717,
477.484522337147));
#14036=CARTESIAN_POINT('Ctrl Pts',(-0.5000512665282,1.22355531214914,478.465534919309));
#14037=CARTESIAN_POINT('Ctrl Pts',(-0.50036909529811,2.30597110420312,478.639497203177));
#14038=CARTESIAN_POINT('Ctrl Pts',(-0.499999999999998,3.13177298256775,
478.650929350314));
#14039=CARTESIAN_POINT('Ctrl Pts',(-0.52515909003033,-0.267385902268368,
476.446209595194));
#14040=CARTESIAN_POINT('Ctrl Pts',(-0.525159090030321,-0.267385902268311,
476.897925674254));
#14041=CARTESIAN_POINT('Ctrl Pts',(-0.528508029696729,-0.00549022311513094,
477.557274036841));
#14042=CARTESIAN_POINT('Ctrl Pts',(-0.545611187563797,1.16274325449317,
478.618027424828));
#14043=CARTESIAN_POINT('Ctrl Pts',(-0.566962243125236,2.28515809867657,
478.826112573076));
#14044=CARTESIAN_POINT('Ctrl Pts',(-0.586829026896253,3.13177298256775,
478.859380568298));
#14045=CARTESIAN_POINT('Ctrl Pts',(-0.595937393540281,-0.361263504246999,
476.446209595194));
#14046=CARTESIAN_POINT('Ctrl Pts',(-0.595937393540267,-0.361263504246951,
476.921954461446));
#14047=CARTESIAN_POINT('Ctrl Pts',(-0.608414354070092,-0.0882434735480379,
477.615790786554));
#14048=CARTESIAN_POINT('Ctrl Pts',(-0.668374925052943,1.12437409329788,
478.725158324453));
#14049=CARTESIAN_POINT('Ctrl Pts',(-0.738643651971611,2.27635772877052,
478.928024760584));
#14050=CARTESIAN_POINT('Ctrl Pts',(-0.795280244880331,3.13177298256775,
478.946209595194));
#14051=CARTESIAN_POINT('Ctrl Pts',(-0.639534883720934,-0.398669801093842,
476.446209595194));
#14052=CARTESIAN_POINT('Ctrl Pts',(-0.639534883720916,-0.398669801093799,
476.93150918906));
#14053=CARTESIAN_POINT('Ctrl Pts',(-0.657106776481008,-0.119751885582937,
477.639104541356));
#14054=CARTESIAN_POINT('Ctrl Pts',(-0.739978110974983,1.11474130806174,
478.759354402431));
#14055=CARTESIAN_POINT('Ctrl Pts',(-0.83207413779171,2.27644192463902,478.946209595194));
#14056=CARTESIAN_POINT('Ctrl Pts',(-0.899999999999989,3.13177298256775,
478.946209595194));
#14057=CARTESIAN_POINT('',(-0.499999999999998,3.13177298256775,478.546209595194));
#14058=CARTESIAN_POINT('Origin',(-0.899999999999999,3.13177298256775,478.546209595194));
#14059=CARTESIAN_POINT('Ctrl Pts',(-0.499999999999998,-0.0950945662644388,
476.446209595194));
#14060=CARTESIAN_POINT('Ctrl Pts',(-0.499999999999998,-0.0950945662643835,
476.853861254042));
#14061=CARTESIAN_POINT('Ctrl Pts',(-0.499999999999998,0.151415578718571,
477.44824134997));
#14062=CARTESIAN_POINT('Ctrl Pts',(-0.499999999999998,1.25403127909223,
478.389251233274));
#14063=CARTESIAN_POINT('Ctrl Pts',(-0.499999999999998,2.31646966486893,
478.546209595194));
#14064=CARTESIAN_POINT('Ctrl Pts',(-0.499999999999998,3.13177298256775,
478.546209595194));
#14065=CARTESIAN_POINT('Origin',(-0.899999999999997,3.07767101631817,478.546209595194));
#14066=CARTESIAN_POINT('',(-0.499999999999997,9.73177298256785,478.546209595194));
#14067=CARTESIAN_POINT('Origin',(-0.899999999999996,9.73177298256785,478.546209595194));
#14068=CARTESIAN_POINT('',(-0.499999999999998,3.07767101631817,478.546209595194));
#14069=CARTESIAN_POINT('Ctrl Pts',(-0.499999999999997,9.73177298256785,
478.546209595194));
#14070=CARTESIAN_POINT('Ctrl Pts',(-0.499999999999997,10.3432782240194,
478.546209595194));
#14071=CARTESIAN_POINT('Ctrl Pts',(-0.499999999999996,11.3741837099334,
478.433754801363));
#14072=CARTESIAN_POINT('Ctrl Pts',(-0.499999999999996,12.6192639795379,
477.649528900673));
#14073=CARTESIAN_POINT('Ctrl Pts',(-0.499999999999996,12.9586405314001,
476.853879756162));
#14074=CARTESIAN_POINT('Ctrl Pts',(-0.499999999999996,12.9586405314001,
476.446209595194));
#14075=CARTESIAN_POINT('Ctrl Pts',(-0.499999999999997,9.73177298256785,
478.650929350314));
#14076=CARTESIAN_POINT('Ctrl Pts',(-0.500276834037699,10.351152501893,478.642354850807));
#14077=CARTESIAN_POINT('Ctrl Pts',(-0.500129097594821,11.4000244981144,
478.513649710999));
#14078=CARTESIAN_POINT('Ctrl Pts',(-0.500256459014652,12.6697035611434,
477.693063832442));
#14079=CARTESIAN_POINT('Ctrl Pts',(-0.499999999999996,13.0160859158435,
476.868575857786));
#14080=CARTESIAN_POINT('Ctrl Pts',(-0.499999999999996,13.0160859158435,
476.446209595194));
#14081=CARTESIAN_POINT('Ctrl Pts',(-0.586829270574883,9.73177298256785,
478.859380324619));
#14082=CARTESIAN_POINT('Ctrl Pts',(-0.571928506475149,10.366762964519,478.83442819575));
#14083=CARTESIAN_POINT('Ctrl Pts',(-0.549705413042954,11.4515432553218,
478.673426882505));
#14084=CARTESIAN_POINT('Ctrl Pts',(-0.52965786150684,12.7705041717072,477.780379022974));
#14085=CARTESIAN_POINT('Ctrl Pts',(-0.525159120540634,13.1309318533804,
476.89794617633));
#14086=CARTESIAN_POINT('Ctrl Pts',(-0.525159120540634,13.1309318533804,
476.446209595194));
#14087=CARTESIAN_POINT('Ctrl Pts',(-0.795280244880335,9.73177298256785,
478.946209595194));
#14088=CARTESIAN_POINT('Ctrl Pts',(-0.752800872271635,10.3733635415159,
478.932570350219));
#14089=CARTESIAN_POINT('Ctrl Pts',(-0.682538179064161,11.4815967780087,
478.780697751043));
#14090=CARTESIAN_POINT('Ctrl Pts',(-0.612727723661889,12.8488399457344,
477.850661022245));
#14091=CARTESIAN_POINT('Ctrl Pts',(-0.595937393540274,13.2248094693827,
476.921976054119));
#14092=CARTESIAN_POINT('Ctrl Pts',(-0.595937393540274,13.2248094693827,
476.446209595194));
#14093=CARTESIAN_POINT('Ctrl Pts',(-0.899999999999995,9.73177298256785,
478.946209595194));
#14094=CARTESIAN_POINT('Ctrl Pts',(-0.849053291126402,10.3733003917485,
478.946209595194));
#14095=CARTESIAN_POINT('Ctrl Pts',(-0.759171292493971,11.4876699669056,
478.812334840633));
#14096=CARTESIAN_POINT('Ctrl Pts',(-0.663255216974702,12.8778553746618,
477.878732577907));
#14097=CARTESIAN_POINT('Ctrl Pts',(-0.639534883720926,13.2622157662295,
476.931531215393));
#14098=CARTESIAN_POINT('Ctrl Pts',(-0.639534883720926,13.2622157662295,
476.446209595194));
#14099=CARTESIAN_POINT('',(-0.499999999999996,12.9586405314001,476.446209595194));
#14100=CARTESIAN_POINT('',(-0.639534883720926,13.2622157662295,476.446209595194));
#14101=CARTESIAN_POINT('Origin',(-0.899999999999996,12.9586405314001,476.446209595194));
#14102=CARTESIAN_POINT('Ctrl Pts',(-0.639534883720926,13.2622157662295,
476.446209595194));
#14103=CARTESIAN_POINT('Ctrl Pts',(-0.639534883720926,13.2622157662295,
476.931531215393));
#14104=CARTESIAN_POINT('Ctrl Pts',(-0.663255216974702,12.8778553746618,
477.878732577907));
#14105=CARTESIAN_POINT('Ctrl Pts',(-0.759171292493971,11.4876699669056,
478.812334840633));
#14106=CARTESIAN_POINT('Ctrl Pts',(-0.849053291126402,10.3733003917485,
478.946209595194));
#14107=CARTESIAN_POINT('Ctrl Pts',(-0.899999999999995,9.73177298256785,
478.946209595194));
#14108=CARTESIAN_POINT('Ctrl Pts',(-0.499999999999997,9.73177298256785,
478.546209595194));
#14109=CARTESIAN_POINT('Ctrl Pts',(-0.499999999999997,10.3432782240194,
478.546209595194));
#14110=CARTESIAN_POINT('Ctrl Pts',(-0.499999999999996,11.3741837099334,
478.433754801363));
#14111=CARTESIAN_POINT('Ctrl Pts',(-0.499999999999996,12.6192639795379,
477.649528900673));
#14112=CARTESIAN_POINT('Ctrl Pts',(-0.499999999999996,12.9586405314001,
476.853879756162));
#14113=CARTESIAN_POINT('Ctrl Pts',(-0.499999999999996,12.9586405314001,
476.446209595194));
#14114=CARTESIAN_POINT('Origin',(-0.899999999999996,12.9586405314001,462.946209595194));
#14115=CARTESIAN_POINT('',(-0.639534883720926,13.2622157662295,462.946209595194));
#14116=CARTESIAN_POINT('',(-0.499999999999996,12.9586405314001,462.946209595194));
#14117=CARTESIAN_POINT('Origin',(-6.5,6.43177298256785,464.546209595194));
#14118=CARTESIAN_POINT('Origin',(-6.5,6.43177298256785,464.546209595194));
#14119=CARTESIAN_POINT('Origin',(-6.5,6.43177298256785,464.946209595194));
#14120=CARTESIAN_POINT('Origin',(-0.0999999999999979,3.07767101631817,465.346209595194));
#14121=CARTESIAN_POINT('',(-0.499999999999998,3.07767101631817,465.346209595194));
#14122=CARTESIAN_POINT('',(-0.0999999999999979,3.07767101631817,464.946209595194));
#14123=CARTESIAN_POINT('Origin',(-6.5,6.43177298256785,462.946209595194));
#14124=CARTESIAN_POINT('Origin',(-6.5,6.43177298256785,476.446209595194));
#14125=CARTESIAN_POINT('',(-15.5,6.43177298256785,463.346209595194));
#14126=CARTESIAN_POINT('',(-15.5,6.43177298256785,462.946209595194));
#14127=CARTESIAN_POINT('Origin',(-6.5,6.43177298256785,463.346209595194));
#14128=CARTESIAN_POINT('Origin',(-0.499999999999998,-0.276430949931514,
478.946209595194));
#14129=CARTESIAN_POINT('',(-0.499999999999999,10.4317729825678,471.090577685893));
#14130=CARTESIAN_POINT('Origin',(-0.499999999999999,6.43177298256785,471.090577685893));
#14131=CARTESIAN_POINT('Origin',(1.,6.43177298256785,464.946209595194));
#14132=CARTESIAN_POINT('Origin',(-6.5,6.43177298256785,476.446209595194));
#14133=CARTESIAN_POINT('Origin',(-6.5,6.43177298256785,463.346209595194));
#14134=CARTESIAN_POINT('',(-15.1,6.43177298256785,462.946209595194));
#14135=CARTESIAN_POINT('Origin',(-15.1,6.43177298256785,463.346209595194));
#14136=CARTESIAN_POINT('Origin',(-6.5,6.43177298256785,462.946209595194));
#14137=CARTESIAN_POINT('Origin',(-6.5,6.43177298256785,462.946209595194));
#14138=CARTESIAN_POINT('',(-13.9,6.43177298256785,462.946209595194));
#14139=CARTESIAN_POINT('Origin',(-6.5,6.43177298256785,462.946209595194));
#14140=CARTESIAN_POINT('Origin',(-6.5,6.43177298256785,462.546209595194));
#14141=CARTESIAN_POINT('',(-13.5,6.43177298256785,462.546209595194));
#14142=CARTESIAN_POINT('Origin',(-6.5,6.43177298256785,462.546209595194));
#14143=CARTESIAN_POINT('Origin',(-13.9,6.43177298256785,462.546209595194));
#14144=CARTESIAN_POINT('Origin',(-6.5,6.43177298256785,462.946209595194));
#14145=CARTESIAN_POINT('',(-13.5,6.43177298256785,451.346209595194));
#14146=CARTESIAN_POINT('',(0.499999999999999,6.43177298256785,451.346209595194));
#14147=CARTESIAN_POINT('Origin',(-6.5,6.43177298256785,451.346209595194));
#14148=CARTESIAN_POINT('',(-13.5,6.43177298256785,462.946209595194));
#14149=CARTESIAN_POINT('Origin',(-6.5,6.43177298256785,451.346209595194));
#14150=CARTESIAN_POINT('Origin',(-6.5,6.43177298256785,451.346209595194));
#14151=CARTESIAN_POINT('',(0.099999999999999,6.43177298256785,450.946209595194));
#14152=CARTESIAN_POINT('Origin',(-6.5,6.43177298256785,450.946209595194));
#14153=CARTESIAN_POINT('Origin',(0.099999999999999,6.43177298256785,451.346209595194));
#14154=CARTESIAN_POINT('Origin',(-6.5,6.43177298256785,450.946209595194));
#14155=CARTESIAN_POINT('',(-12.5,6.43177298256785,450.946209595194));
#14156=CARTESIAN_POINT('Origin',(-6.5,6.43177298256785,450.946209595194));
#14157=CARTESIAN_POINT('Origin',(-6.5,6.43177298256785,451.446209595194));
#14158=CARTESIAN_POINT('',(-11.5,6.43177298256785,451.946209595194));
#14159=CARTESIAN_POINT('',(-12.,6.43177298256785,451.446209595194));
#14160=CARTESIAN_POINT('Origin',(-6.5,6.43177298256785,451.946209595194));
#14161=CARTESIAN_POINT('Origin',(-6.5,6.43177298256785,462.946209595194));
#14162=CARTESIAN_POINT('',(-11.5,6.43177298256785,462.946209595194));
#14163=CARTESIAN_POINT('',(-11.5,6.43177298256785,462.946209595194));
#14164=CARTESIAN_POINT('Origin',(-6.5,6.43177298256785,462.946209595194));
#14165=CARTESIAN_POINT('Origin',(-12.5,6.43177298256785,471.090577685893));
#14166=CARTESIAN_POINT('',(-12.5,10.4317729825678,471.090577685893));
#14167=CARTESIAN_POINT('Origin',(-6.5,6.43177298256785,462.946209595194));
#14168=CARTESIAN_POINT('',(0.,0.,0.));
#14169=CARTESIAN_POINT('Origin',(-6.5,6.43177298256785,260.886209595194));
#14170=CARTESIAN_POINT('',(-15.3655563966863,6.43160863162147,258.077824816097));
#14171=CARTESIAN_POINT('',(-15.3658820331401,6.43164402321515,258.444594374291));
#14172=CARTESIAN_POINT('',(-15.366,6.43177298256785,260.886209595194));
#14173=CARTESIAN_POINT('',(-2.55683773519921,-1.50909770983428,258.886209595194));
#14174=CARTESIAN_POINT('Ctrl Pts',(-15.3655563966863,6.43160863162147,258.077824816097));
#14175=CARTESIAN_POINT('Ctrl Pts',(-15.365908581386,5.92277029184256,258.100657338524));
#14176=CARTESIAN_POINT('Ctrl Pts',(-15.3227955907809,5.41399103993066,258.123489860952));
#14177=CARTESIAN_POINT('Ctrl Pts',(-15.2356628566919,4.91286580948705,258.146322383379));
#14178=CARTESIAN_POINT('Ctrl Pts',(-14.9876098477437,3.48624213503058,258.211322936263));
#14179=CARTESIAN_POINT('Ctrl Pts',(-14.382798754648,2.12165049027129,258.276323489146));
#14180=CARTESIAN_POINT('Ctrl Pts',(-13.4924209785142,0.979715202365416,
258.341324042029));
#14181=CARTESIAN_POINT('Ctrl Pts',(-12.6020432023805,-0.162220085540456,
258.406324594912));
#14182=CARTESIAN_POINT('Ctrl Pts',(-11.4260987432086,-1.08149901659292,
258.471325147796));
#14183=CARTESIAN_POINT('Ctrl Pts',(-10.1030119047582,-1.66990669415313,
258.536325700679));
#14184=CARTESIAN_POINT('Ctrl Pts',(-8.77992506630778,-2.25831437171335,
258.601326253562));
#14185=CARTESIAN_POINT('Ctrl Pts',(-7.30969584857881,-2.51585079578131,
258.666326806446));
#14186=CARTESIAN_POINT('Ctrl Pts',(-5.86537969542476,-2.41221435349705,
258.731327359329));
#14187=CARTESIAN_POINT('Ctrl Pts',(-4.71821552951209,-2.3298999567415,258.782954771284));
#14188=CARTESIAN_POINT('Ctrl Pts',(-3.58739863923219,-2.01973939457909,
258.834582183239));
#14189=CARTESIAN_POINT('Ctrl Pts',(-2.55659399163549,-1.50913350781768,
258.886209595194));
#14190=CARTESIAN_POINT('',(-10.4431622648008,-1.50909770983426,258.886209595194));
#14191=CARTESIAN_POINT('Origin',(-6.5,6.43177298256785,258.886209595194));
#14192=CARTESIAN_POINT('Ctrl Pts',(-10.4431622648007,-1.50909770983434,
258.886209595194));
#14193=CARTESIAN_POINT('Ctrl Pts',(-11.7404163125939,-0.86492613126773,
258.82120904231));
#14194=CARTESIAN_POINT('Ctrl Pts',(-12.8761753779444,0.10296746655448,258.756208489427));
#14195=CARTESIAN_POINT('Ctrl Pts',(-13.7172937557503,1.28146572034169,258.691207936544));
#14196=CARTESIAN_POINT('Ctrl Pts',(-14.5584121335561,2.4599639741289,258.626207383661));
#14197=CARTESIAN_POINT('Ctrl Pts',(-15.1048898238173,3.84906688388111,258.561206830778));
#14198=CARTESIAN_POINT('Ctrl Pts',(-15.2922292071869,5.28493656649312,258.496206277894));
#14199=CARTESIAN_POINT('Ctrl Pts',(-15.3418131043833,5.66497419365675,258.479002310026));
#14200=CARTESIAN_POINT('Ctrl Pts',(-15.3662384939932,6.04828794644444,258.461798342159));
#14201=CARTESIAN_POINT('Ctrl Pts',(-15.3658820331401,6.43164402321515,258.444594374291));
#14202=CARTESIAN_POINT('Origin',(-6.5,6.43177298256785,260.886209595194));
#14203=CARTESIAN_POINT('',(-15.3662755781924,6.43158183962034,255.577824816097));
#14204=CARTESIAN_POINT('',(-15.3665939393721,6.43165874093672,255.944594374291));
#14205=CARTESIAN_POINT('',(-15.366,6.43177298256785,260.886209595194));
#14206=CARTESIAN_POINT('Ctrl Pts',(-15.3662755781924,6.43158183962034,255.577824816097));
#14207=CARTESIAN_POINT('Ctrl Pts',(-15.3665112565053,6.1829613866446,255.588983484375));
#14208=CARTESIAN_POINT('Ctrl Pts',(-15.3562554254084,5.93436031665608,255.600142152654));
#14209=CARTESIAN_POINT('Ctrl Pts',(-15.3353656673878,5.68665604249679,255.611300820932));
#14210=CARTESIAN_POINT('Ctrl Pts',(-15.213680374209,4.2437495620628,255.676301373815));
#14211=CARTESIAN_POINT('Ctrl Pts',(-14.7311647485395,2.83127315130671,255.741301926699));
#14212=CARTESIAN_POINT('Ctrl Pts',(-13.9446160597533,1.61549044790784,255.806302479582));
#14213=CARTESIAN_POINT('Ctrl Pts',(-13.158067370967,0.399707744508963,255.871303032465));
#14214=CARTESIAN_POINT('Ctrl Pts',(-12.067485619064,-0.619381251532671,
255.936303585348));
#14215=CARTESIAN_POINT('Ctrl Pts',(-10.8012439843536,-1.32181882492555,
256.001304138232));
#14216=CARTESIAN_POINT('Ctrl Pts',(-9.53500234964327,-2.02425639831843,
256.066304691115));
#14217=CARTESIAN_POINT('Ctrl Pts',(-8.0931008321256,-2.41004254906253,256.131305243998));
#14218=CARTESIAN_POINT('Ctrl Pts',(-6.64526672060094,-2.43376610496901,
256.196305796881));
#14219=CARTESIAN_POINT('Ctrl Pts',(-5.19743260907629,-2.45748966087549,
256.261306349765));
#14220=CARTESIAN_POINT('Ctrl Pts',(-3.74366590354462,-2.11915062194435,
256.326306902648));
#14221=CARTESIAN_POINT('Ctrl Pts',(-2.45509055196917,-1.4585751265513,256.391307455531));
#14222=CARTESIAN_POINT('Ctrl Pts',(-1.16651520039374,-0.797999631158263,
256.456308008415));
#14223=CARTESIAN_POINT('Ctrl Pts',(-0.0431312027745352,0.184812320696678,
256.521308561298));
#14224=CARTESIAN_POINT('Ctrl Pts',(0.782827082714929,1.37417321356813,256.586309114181));
#14225=CARTESIAN_POINT('Ctrl Pts',(1.6087853682044,2.5635341064396,256.651309667064));
#14226=CARTESIAN_POINT('Ctrl Pts',(2.13731794156413,3.95944394032759,256.716310219948));
#14227=CARTESIAN_POINT('Ctrl Pts',(2.30621084745112,5.39758913611839,256.781310772831));
#14228=CARTESIAN_POINT('Ctrl Pts',(2.47510375333811,6.83573433190919,256.846311325714));
#14229=CARTESIAN_POINT('Ctrl Pts',(2.28435699175236,8.31611488960281,256.911311878597));
#14230=CARTESIAN_POINT('Ctrl Pts',(1.75642349837671,9.66447413648814,256.976312431481));
#14231=CARTESIAN_POINT('Ctrl Pts',(1.22849000500107,11.0128333833735,257.041312984364));
#14232=CARTESIAN_POINT('Ctrl Pts',(0.363369779835524,12.2291713194505,257.106313537247));
#14233=CARTESIAN_POINT('Ctrl Pts',(-0.737103225919464,13.1703118853259,
257.17131409013));
#14234=CARTESIAN_POINT('Ctrl Pts',(-1.83757623167446,14.1114524512014,257.236314643014));
#14235=CARTESIAN_POINT('Ctrl Pts',(-3.1734020180189,14.7773956468752,257.301315195897));
#14236=CARTESIAN_POINT('Ctrl Pts',(-4.58733957700001,15.0897528652687,257.36631574878));
#14237=CARTESIAN_POINT('Ctrl Pts',(-6.00127713598111,15.4021100836622,257.431316301664));
#14238=CARTESIAN_POINT('Ctrl Pts',(-7.49332646759887,15.3608813247754,257.496316854547));
#14239=CARTESIAN_POINT('Ctrl Pts',(-8.88785728598738,14.9709195332554,257.56131740743));
#14240=CARTESIAN_POINT('Ctrl Pts',(-10.2823881043759,14.5809577417353,257.626317960313));
#14241=CARTESIAN_POINT('Ctrl Pts',(-11.5794004095351,13.842262917582,257.691318513197));
#14242=CARTESIAN_POINT('Ctrl Pts',(-12.626222062206,12.8417876386424,257.75631906608));
#14243=CARTESIAN_POINT('Ctrl Pts',(-13.6730437148769,11.8413123597028,257.821319618963));
#14244=CARTESIAN_POINT('Ctrl Pts',(-14.4696747150594,10.5790566259768,257.886320171846));
#14245=CARTESIAN_POINT('Ctrl Pts',(-14.9223427527502,9.20360090703698,257.951320724729));
#14246=CARTESIAN_POINT('Ctrl Pts',(-15.2160036333582,8.31129682539304,257.993488755185));
#14247=CARTESIAN_POINT('Ctrl Pts',(-15.3649059676683,7.37135195945706,258.035656785641));
#14248=CARTESIAN_POINT('Ctrl Pts',(-15.3655563966863,6.43160863162147,258.077824816097));
#14249=CARTESIAN_POINT('Ctrl Pts',(-15.3658820331401,6.43164402321515,258.444594374291));
#14250=CARTESIAN_POINT('Ctrl Pts',(-15.3648917027932,7.49669549595043,258.396797789275));
#14251=CARTESIAN_POINT('Ctrl Pts',(-15.1726210818878,8.56207364904321,258.34900120426));
#14252=CARTESIAN_POINT('Ctrl Pts',(-14.7971471860228,9.55843300974454,258.301204619244));
#14253=CARTESIAN_POINT('Ctrl Pts',(-14.286524705011,10.9134233149121,258.236204066361));
#14254=CARTESIAN_POINT('Ctrl Pts',(-13.4370786665095,12.1407674697755,258.171203513478));
#14255=CARTESIAN_POINT('Ctrl Pts',(-12.3487596071053,13.0959348658895,258.106202960595));
#14256=CARTESIAN_POINT('Ctrl Pts',(-11.2604405477011,14.0511022620034,258.041202407711));
#14257=CARTESIAN_POINT('Ctrl Pts',(-9.93324846739419,14.734092899368,257.976201854828));
#14258=CARTESIAN_POINT('Ctrl Pts',(-8.52342686227239,15.0645361066618,257.911201301945));
#14259=CARTESIAN_POINT('Ctrl Pts',(-7.11360525715061,15.3949793139555,257.846200749062));
#14260=CARTESIAN_POINT('Ctrl Pts',(-5.6211541272139,15.3728750911786,257.781200196178));
#14261=CARTESIAN_POINT('Ctrl Pts',(-4.22174266980788,15.0008133213866,257.716199643295));
#14262=CARTESIAN_POINT('Ctrl Pts',(-2.82233121240186,14.6287515515946,257.651199090412));
#14263=CARTESIAN_POINT('Ctrl Pts',(-1.51595942752651,13.9067322347875,257.586198537529));
#14264=CARTESIAN_POINT('Ctrl Pts',(-0.456405209262731,12.919750140243,257.521197984645));
#14265=CARTESIAN_POINT('Ctrl Pts',(0.603149009001058,11.9327680456984,257.456197431762));
#14266=CARTESIAN_POINT('Ctrl Pts',(1.41588566065329,10.6808231734162,257.391196878879));
#14267=CARTESIAN_POINT('Ctrl Pts',(1.88613869287802,9.31128036624651,257.326196325996));
#14268=CARTESIAN_POINT('Ctrl Pts',(2.35639172510274,7.94173755907686,257.261195773112));
#14269=CARTESIAN_POINT('Ctrl Pts',(2.48416113789998,6.45459681701972,257.196195220229));
#14270=CARTESIAN_POINT('Ctrl Pts',(2.25440627641291,5.024911711378,257.131194667346));
#14271=CARTESIAN_POINT('Ctrl Pts',(2.02465141492584,3.59522660573629,257.066194114462));
#14272=CARTESIAN_POINT('Ctrl Pts',(1.43737227915447,2.22299713651001,257.001193561579));
#14273=CARTESIAN_POINT('Ctrl Pts',(0.561698305318104,1.06974891578268,256.936193008696));
#14274=CARTESIAN_POINT('Ctrl Pts',(-0.313975668518257,-0.0834993049446531,
256.871192455813));
#14275=CARTESIAN_POINT('Ctrl Pts',(-1.47804448041961,-1.01776627717304,
256.806191902929));
#14276=CARTESIAN_POINT('Ctrl Pts',(-2.79348490795269,-1.62307850617608,
256.741191350046));
#14277=CARTESIAN_POINT('Ctrl Pts',(-4.10892533548576,-2.22839073517912,
256.676190797163));
#14278=CARTESIAN_POINT('Ctrl Pts',(-5.57573737865058,-2.50474822095681,
256.61119024428));
#14279=CARTESIAN_POINT('Ctrl Pts',(-7.02126143274018,-2.41962083214006,
256.546189691396));
#14280=CARTESIAN_POINT('Ctrl Pts',(-8.46678548682979,-2.33449344332332,
256.481189138513));
#14281=CARTESIAN_POINT('Ctrl Pts',(-9.8910215518442,-1.88788117991214,256.41618858563));
#14282=CARTESIAN_POINT('Ctrl Pts',(-11.1263217894382,-1.13235504876889,
256.351188032747));
#14283=CARTESIAN_POINT('Ctrl Pts',(-12.3616220270321,-0.37682891762563,
256.286187479863));
#14284=CARTESIAN_POINT('Ctrl Pts',(-13.4079864372057,0.687611081249703,
256.22118692698));
#14285=CARTESIAN_POINT('Ctrl Pts',(-14.1422466784471,1.93566890880313,256.156186374097));
#14286=CARTESIAN_POINT('Ctrl Pts',(-14.8765069196884,3.18372673635655,256.091185821213));
#14287=CARTESIAN_POINT('Ctrl Pts',(-15.2986629919977,4.61540239258807,256.02618526833));
#14288=CARTESIAN_POINT('Ctrl Pts',(-15.3590226012745,6.06217229347312,255.961184715447));
#14289=CARTESIAN_POINT('Ctrl Pts',(-15.3641578730301,6.18526050921736,255.955654601728));
#14290=CARTESIAN_POINT('Ctrl Pts',(-15.3666743688619,6.30845798098958,255.950124488009));
#14291=CARTESIAN_POINT('Ctrl Pts',(-15.3665939393721,6.43165874093672,255.944594374291));
#14292=CARTESIAN_POINT('Origin',(-6.5,6.43177298256785,260.886209595194));
#14293=CARTESIAN_POINT('',(-15.3667277726507,6.43178433461072,253.077824816097));
#14294=CARTESIAN_POINT('',(-15.3665655929379,6.43189805357513,253.444594374291));
#14295=CARTESIAN_POINT('',(-15.366,6.43177298256785,260.886209595194));
#14296=CARTESIAN_POINT('Ctrl Pts',(-15.3667277726507,6.43178433461072,253.077824816097));
#14297=CARTESIAN_POINT('Ctrl Pts',(-15.3666159753282,4.99523210882893,253.14231018311));
#14298=CARTESIAN_POINT('Ctrl Pts',(-15.0104403492592,3.55862641061937,253.206795550122));
#14299=CARTESIAN_POINT('Ctrl Pts',(-14.3391729900672,2.2885553244482,253.271280917135));
#14300=CARTESIAN_POINT('Ctrl Pts',(-13.662542748179,1.00833739863445,253.336281470018));
#14301=CARTESIAN_POINT('Ctrl Pts',(-12.6657660061007,-0.102674332284354,
253.401282022901));
#14302=CARTESIAN_POINT('Ctrl Pts',(-11.4661740875396,-0.913701860014089,
253.466282575784));
#14303=CARTESIAN_POINT('Ctrl Pts',(-10.2665821689785,-1.72472938774381,
253.531283128668));
#14304=CARTESIAN_POINT('Ctrl Pts',(-8.86417507393453,-2.23577271228447,
253.596283681551));
#14305=CARTESIAN_POINT('Ctrl Pts',(-7.42403117341256,-2.38667654789474,
253.661284234434));
#14306=CARTESIAN_POINT('Ctrl Pts',(-5.98388727289058,-2.537580383505,253.726284787317));
#14307=CARTESIAN_POINT('Ctrl Pts',(-4.50600656689059,-2.32834473018485,
253.791285340201));
#14308=CARTESIAN_POINT('Ctrl Pts',(-3.16435148069425,-1.78359887063561,
253.856285893084));
#14309=CARTESIAN_POINT('Ctrl Pts',(-1.8226963944979,-1.23885301108636,253.921286445967));
#14310=CARTESIAN_POINT('Ctrl Pts',(-0.617266928105228,-0.358596945308037,
253.986286998851));
#14311=CARTESIAN_POINT('Ctrl Pts',(0.31004492907752,0.753553737531672,254.051287551734));
#14312=CARTESIAN_POINT('Ctrl Pts',(1.23735678626026,1.86570442037137,254.116288104617));
#14313=CARTESIAN_POINT('Ctrl Pts',(1.88655103423305,3.20974972027245,254.1812886575));
#14314=CARTESIAN_POINT('Ctrl Pts',(2.18121054041009,4.62748107607727,254.246289210384));
#14315=CARTESIAN_POINT('Ctrl Pts',(2.47587004658713,6.04521243188211,254.311289763267));
#14316=CARTESIAN_POINT('Ctrl Pts',(2.41599481096842,7.53662984359073,254.37629031615));
#14317=CARTESIAN_POINT('Ctrl Pts',(2.0086327915932,8.92617747033215,254.441290869033));
#14318=CARTESIAN_POINT('Ctrl Pts',(1.60127077221798,10.3157250970736,254.506291421917));
#14319=CARTESIAN_POINT('Ctrl Pts',(0.846421969086256,11.6034029388478,254.5712919748));
#14320=CARTESIAN_POINT('Ctrl Pts',(-0.16705980979175,12.6376374894676,254.636292527683));
#14321=CARTESIAN_POINT('Ctrl Pts',(-1.18054158866975,13.6718720400874,254.701293080566));
#14322=CARTESIAN_POINT('Ctrl Pts',(-2.45265634329403,14.4526632995527,254.76629363345));
#14323=CARTESIAN_POINT('Ctrl Pts',(-3.83366250991437,14.8881037542279,254.831294186333));
#14324=CARTESIAN_POINT('Ctrl Pts',(-5.21466867653472,15.3235442089031,254.896294739216));
#14325=CARTESIAN_POINT('Ctrl Pts',(-6.70456625515113,15.4136338587881,254.9612952921));
#14326=CARTESIAN_POINT('Ctrl Pts',(-8.12797830556721,15.1477681849149,255.026295844983));
#14327=CARTESIAN_POINT('Ctrl Pts',(-9.55139035598328,14.8819025110416,255.091296397866));
#14328=CARTESIAN_POINT('Ctrl Pts',(-10.908316878199,14.2600815134102,255.156296950749));
#14329=CARTESIAN_POINT('Ctrl Pts',(-12.0390330528948,13.3555001991571,255.221297503632));
#14330=CARTESIAN_POINT('Ctrl Pts',(-13.1697492275906,12.450918884904,255.286298056516));
#14331=CARTESIAN_POINT('Ctrl Pts',(-14.0742550547665,11.2635772540293,255.351298609399));
#14332=CARTESIAN_POINT('Ctrl Pts',(-14.6460804880105,9.93323816353598,255.416299162282));
#14333=CARTESIAN_POINT('Ctrl Pts',(-15.1197404435826,8.83127886290768,255.470141046887));
#14334=CARTESIAN_POINT('Ctrl Pts',(-15.3651384026615,7.63120471625482,255.523982931492));
#14335=CARTESIAN_POINT('Ctrl Pts',(-15.3662755781924,6.43158183962034,255.577824816097));
#14336=CARTESIAN_POINT('Ctrl Pts',(-15.3665939393721,6.43165874093672,255.944594374291));
#14337=CARTESIAN_POINT('Ctrl Pts',(-15.3657290065113,7.75655071821844,255.885123935126));
#14338=CARTESIAN_POINT('Ctrl Pts',(-15.0645375921236,9.08182296288714,255.825653495962));
#14339=CARTESIAN_POINT('Ctrl Pts',(-14.4901943902724,10.2756876209297,255.766183056797));
#14340=CARTESIAN_POINT('Ctrl Pts',(-13.8624434237493,11.5805689019627,255.701182503914));
#14341=CARTESIAN_POINT('Ctrl Pts',(-12.9083783444587,12.7284673184901,255.636181951031));
#14342=CARTESIAN_POINT('Ctrl Pts',(-11.7403028565014,13.5842629056116,255.571181398147));
#14343=CARTESIAN_POINT('Ctrl Pts',(-10.5722273685442,14.440058492733,255.506180845264));
#14344=CARTESIAN_POINT('Ctrl Pts',(-9.19014147192026,15.0037512504485,255.441180292381));
#14345=CARTESIAN_POINT('Ctrl Pts',(-7.75673151365957,15.2089884884431,255.376179739498));
#14346=CARTESIAN_POINT('Ctrl Pts',(-6.32332155539888,15.4142257264378,255.311179186614));
#14347=CARTESIAN_POINT('Ctrl Pts',(-4.83858753550142,15.2610074447117,255.246178633731));
#14348=CARTESIAN_POINT('Ctrl Pts',(-3.47729858821851,14.767369080426,255.181178080848));
#14349=CARTESIAN_POINT('Ctrl Pts',(-2.11600964093561,14.2737307161403,255.116177527965));
#14350=CARTESIAN_POINT('Ctrl Pts',(-0.878165766267253,13.4396722692951,
255.051176975081));
#14351=CARTESIAN_POINT('Ctrl Pts',(0.0905255226928164,12.3633713731189,
254.986176422198));
#14352=CARTESIAN_POINT('Ctrl Pts',(1.05921681165288,11.2870704769428,254.921175869315));
#14353=CARTESIAN_POINT('Ctrl Pts',(1.75875551490466,9.96852713143572,254.856175316432));
#14354=CARTESIAN_POINT('Ctrl Pts',(2.10679841691598,8.56294804404318,254.791174763548));
#14355=CARTESIAN_POINT('Ctrl Pts',(2.4548413189273,7.15736895665064,254.726174210665));
#14356=CARTESIAN_POINT('Ctrl Pts',(2.45138841969816,5.6647541273726,254.661173657782));
#14357=CARTESIAN_POINT('Ctrl Pts',(2.09684616257126,4.26080034593536,254.596173104898));
#14358=CARTESIAN_POINT('Ctrl Pts',(1.74230390544437,2.85684656449812,254.531172552015));
#14359=CARTESIAN_POINT('Ctrl Pts',(1.03667229041973,1.54155383090168,254.466171999132));
#14360=CARTESIAN_POINT('Ctrl Pts',(0.0630117340679463,0.469746220590651,
254.401171446249));
#14361=CARTESIAN_POINT('Ctrl Pts',(-0.910648822283835,-0.602061389720375,
254.336170893365));
#14362=CARTESIAN_POINT('Ctrl Pts',(-2.15233831996276,-1.43038387674599,
254.271170340482));
#14363=CARTESIAN_POINT('Ctrl Pts',(-3.5158965745936,-1.91771879109464,254.206169787599));
#14364=CARTESIAN_POINT('Ctrl Pts',(-4.87945482922443,-2.4050537054433,254.141169234716));
#14365=CARTESIAN_POINT('Ctrl Pts',(-6.36488184080717,-2.55140104711501,
254.076168681832));
#14366=CARTESIAN_POINT('Ctrl Pts',(-7.79732690288103,-2.33953416283919,
254.011168128949));
#14367=CARTESIAN_POINT('Ctrl Pts',(-9.22977196495487,-2.12766727856337,
253.946167576066));
#14368=CARTESIAN_POINT('Ctrl Pts',(-10.6092350775198,-1.55758616834003,
253.881167023183));
#14369=CARTESIAN_POINT('Ctrl Pts',(-11.7733386226286,-0.696395499103504,
253.816166470299));
#14370=CARTESIAN_POINT('Ctrl Pts',(-12.9374421677373,0.164795170133028,
253.751165917416));
#14371=CARTESIAN_POINT('Ctrl Pts',(-13.8861861453898,1.31709539838274,253.686165364533));
#14372=CARTESIAN_POINT('Ctrl Pts',(-14.5078932039212,2.6248670779529,253.62116481165));
#14373=CARTESIAN_POINT('Ctrl Pts',(-15.0708375808772,3.8090304282859,253.562307999197));
#14374=CARTESIAN_POINT('Ctrl Pts',(-15.3656453212045,5.12066437784316,253.503451186744));
#14375=CARTESIAN_POINT('Ctrl Pts',(-15.3665655929379,6.43189805357513,253.444594374291));
#14376=CARTESIAN_POINT('Origin',(-6.5,6.43177298256785,260.886209595194));
#14377=CARTESIAN_POINT('',(-15.3662080510474,6.43197208529678,250.577824816097));
#14378=CARTESIAN_POINT('',(-15.3658371696729,6.43197914685562,250.944594374291));
#14379=CARTESIAN_POINT('',(-15.366,6.43177298256785,260.886209595194));
#14380=CARTESIAN_POINT('Ctrl Pts',(-15.3662080510474,6.43197208529678,250.577824816097));
#14381=CARTESIAN_POINT('Ctrl Pts',(-15.365069838388,5.25528049615197,250.63063632896));
#14382=CARTESIAN_POINT('Ctrl Pts',(-15.1292211412892,4.07814608026942,250.683447841824));
#14383=CARTESIAN_POINT('Ctrl Pts',(-14.6730366414472,2.99369826140245,250.736259354687));
#14384=CARTESIAN_POINT('Ctrl Pts',(-14.1115635250993,1.65895695259718,250.801259907571));
#14385=CARTESIAN_POINT('Ctrl Pts',(-13.2163091438145,0.464624280106945,
250.866260460454));
#14386=CARTESIAN_POINT('Ctrl Pts',(-12.0926545495139,-0.448713978436843,
250.931261013337));
#14387=CARTESIAN_POINT('Ctrl Pts',(-10.9689999552133,-1.36205223698062,
250.996261566221));
#14388=CARTESIAN_POINT('Ctrl Pts',(-9.61694514789703,-1.99439608157795,
251.061262119104));
#14389=CARTESIAN_POINT('Ctrl Pts',(-8.19564149373379,-2.27131185302248,
251.126262671987));
#14390=CARTESIAN_POINT('Ctrl Pts',(-6.77433783957052,-2.54822762446701,
251.19126322487));
#14391=CARTESIAN_POINT('Ctrl Pts',(-5.2837853385603,-2.46971532275872,251.256263777754));
#14392=CARTESIAN_POINT('Ctrl Pts',(-3.89943802229893,-2.0450166886986,251.321264330637));
#14393=CARTESIAN_POINT('Ctrl Pts',(-2.51509070603756,-1.62031805463848,
251.38626488352));
#14394=CARTESIAN_POINT('Ctrl Pts',(-1.23694857452505,-0.849433088226517,
251.451265436403));
#14395=CARTESIAN_POINT('Ctrl Pts',(-0.215462678478693,0.1768967739479,251.516265989287));
#14396=CARTESIAN_POINT('Ctrl Pts',(0.806023217567654,1.20322663612231,251.58126654217));
#14397=CARTESIAN_POINT('Ctrl Pts',(1.57085287814786,2.4850013940592,251.646267095053));
#14398=CARTESIAN_POINT('Ctrl Pts',(1.98899764117726,3.87134239791202,251.711267647936));
#14399=CARTESIAN_POINT('Ctrl Pts',(2.40714240420666,5.25768340176484,251.77626820082));
#14400=CARTESIAN_POINT('Ctrl Pts',(2.47860226968529,6.74859065153357,251.841268753703));
#14401=CARTESIAN_POINT('Ctrl Pts',(2.19496564426971,8.16856835788513,251.906269306586));
#14402=CARTESIAN_POINT('Ctrl Pts',(1.91132901885414,9.58854606423668,251.971269859469));
#14403=CARTESIAN_POINT('Ctrl Pts',(1.27259590254435,10.937594227171,252.036270412353));
#14404=CARTESIAN_POINT('Ctrl Pts',(0.353952040421027,12.0569153948417,252.101270965236));
#14405=CARTESIAN_POINT('Ctrl Pts',(-0.564691821702289,13.1762365625124,
252.166271518119));
#14406=CARTESIAN_POINT('Ctrl Pts',(-1.76324642963914,14.0658307349195,252.231272071002));
#14407=CARTESIAN_POINT('Ctrl Pts',(-3.10062903863032,14.6209831274933,252.296272623886));
#14408=CARTESIAN_POINT('Ctrl Pts',(-4.43801164762152,15.1761355200672,252.361273176769));
#14409=CARTESIAN_POINT('Ctrl Pts',(-5.91422225766704,15.3968461328078,252.426273729652));
#14410=CARTESIAN_POINT('Ctrl Pts',(-7.35549503170888,15.2571349570976,252.491274282535));
#14411=CARTESIAN_POINT('Ctrl Pts',(-8.7967678057507,15.1174237813874,252.556274835419));
#14412=CARTESIAN_POINT('Ctrl Pts',(-10.2031027437888,14.6172908172262,252.621275388302));
#14413=CARTESIAN_POINT('Ctrl Pts',(-11.4089591255296,13.8156070838078,252.686275941185));
#14414=CARTESIAN_POINT('Ctrl Pts',(-12.6148155072703,13.0139233503894,252.751276494069));
#14415=CARTESIAN_POINT('Ctrl Pts',(-13.6201933327137,11.9106888477137,252.816277046952));
#14416=CARTESIAN_POINT('Ctrl Pts',(-14.3067488383011,10.6357661208161,252.881277599835));
#14417=CARTESIAN_POINT('Ctrl Pts',(-14.9933043438886,9.36084339391843,252.946278152718));
#14418=CARTESIAN_POINT('Ctrl Pts',(-15.3610375296202,7.91423244279888,253.011278705602));
#14419=CARTESIAN_POINT('Ctrl Pts',(-15.3666622516369,6.46621490688475,253.076279258485));
#14420=CARTESIAN_POINT('Ctrl Pts',(-15.3667068324471,6.45473810950495,253.076794444356));
#14421=CARTESIAN_POINT('Ctrl Pts',(-15.3667286658208,6.44326122376433,253.077309630226));
#14422=CARTESIAN_POINT('Ctrl Pts',(-15.3667277726507,6.43178433461072,253.077824816097));
#14423=CARTESIAN_POINT('Ctrl Pts',(-15.3665655929379,6.43189805357513,253.444594374291));
#14424=CARTESIAN_POINT('Ctrl Pts',(-15.3666616550659,6.5687705584125,253.43845063386));
#14425=CARTESIAN_POINT('Ctrl Pts',(-15.363555481387,6.70563870181459,253.43230689343));
#14426=CARTESIAN_POINT('Ctrl Pts',(-15.3572177832327,6.84235704507857,253.426163153));
#14427=CARTESIAN_POINT('Ctrl Pts',(-15.2901651646025,8.28883220174352,253.361162600116));
#14428=CARTESIAN_POINT('Ctrl Pts',(-14.8613897879318,9.71853938418283,253.296162047233));
#14429=CARTESIAN_POINT('Ctrl Pts',(-14.1213631182881,10.963186708018,253.23116149435));
#14430=CARTESIAN_POINT('Ctrl Pts',(-13.3813364486445,12.2078340318531,253.166160941467));
#14431=CARTESIAN_POINT('Ctrl Pts',(-12.3300584860279,13.2674214970841,253.101160388583));
#14432=CARTESIAN_POINT('Ctrl Pts',(-11.0912759329153,14.0172242835672,253.0361598357));
#14433=CARTESIAN_POINT('Ctrl Pts',(-9.85249337980274,14.7670270700503,252.971159282817));
#14434=CARTESIAN_POINT('Ctrl Pts',(-8.4262062361942,15.2070451777856,252.906158729934));
#14435=CARTESIAN_POINT('Ctrl Pts',(-6.98030381118131,15.2854837515599,252.84115817705));
#14436=CARTESIAN_POINT('Ctrl Pts',(-5.53440138616842,15.3639223253342,252.776157624167));
#14437=CARTESIAN_POINT('Ctrl Pts',(-4.06888367975118,15.0807813651476,252.711157071284));
#14438=CARTESIAN_POINT('Ctrl Pts',(-2.756257859434,14.4693896017499,252.646156518401));
#14439=CARTESIAN_POINT('Ctrl Pts',(-1.44363203911683,13.8579978383522,252.581155965517));
#14440=CARTESIAN_POINT('Ctrl Pts',(-0.283898104899725,12.9183552717433,
252.516155412634));
#14441=CARTESIAN_POINT('Ctrl Pts',(0.586430808524681,11.7610679197985,252.451154859751));
#14442=CARTESIAN_POINT('Ctrl Pts',(1.45675972194909,10.6037805678537,252.386154306867));
#14443=CARTESIAN_POINT('Ctrl Pts',(2.03768361458079,9.22884843057297,252.321153753984));
#14444=CARTESIAN_POINT('Ctrl Pts',(2.2608215075925,7.79811578146756,252.256153201101));
#14445=CARTESIAN_POINT('Ctrl Pts',(2.48395940060421,6.36738313236216,252.191152648218));
#14446=CARTESIAN_POINT('Ctrl Pts',(2.34931129399593,4.88084997143212,252.126152095335));
#14447=CARTESIAN_POINT('Ctrl Pts',(1.87272671546639,3.5134972107951,252.061151542451));
#14448=CARTESIAN_POINT('Ctrl Pts',(1.39614213693684,2.14614445015806,251.996150989568));
#14449=CARTESIAN_POINT('Ctrl Pts',(0.577621086486011,0.897972089814032,
251.931150436685));
#14450=CARTESIAN_POINT('Ctrl Pts',(-0.486487720795355,-0.0840965833347244,
251.866149883801));
#14451=CARTESIAN_POINT('Ctrl Pts',(-1.55059652807671,-1.06616525648347,
251.801149330918));
#14452=CARTESIAN_POINT('Ctrl Pts',(-2.86029309218863,-1.78213024243697,
251.736148778035));
#14453=CARTESIAN_POINT('Ctrl Pts',(-4.26141206693571,-2.14771477591397,
251.671148225152));
#14454=CARTESIAN_POINT('Ctrl Pts',(-5.6625310416828,-2.51329930939097,251.606147672268));
#14455=CARTESIAN_POINT('Ctrl Pts',(-7.15507242706507,-2.52850339039149,
251.541147119385));
#14456=CARTESIAN_POINT('Ctrl Pts',(-8.56334807844394,-2.19153733535427,
251.476146566502));
#14457=CARTESIAN_POINT('Ctrl Pts',(-9.9716237298228,-1.85457128031705,251.411146013619));
#14458=CARTESIAN_POINT('Ctrl Pts',(-11.2956336471983,-1.1654350892421,251.346145460735));
#14459=CARTESIAN_POINT('Ctrl Pts',(-12.379527649031,-0.205247490225679,
251.281144907852));
#14460=CARTESIAN_POINT('Ctrl Pts',(-13.4634216508637,0.754940108790739,
251.216144354969));
#14461=CARTESIAN_POINT('Ctrl Pts',(-14.3071997371537,1.98617911574862,251.151143802085));
#14462=CARTESIAN_POINT('Ctrl Pts',(-14.8115401685383,3.34353948123183,251.086143249202));
#14463=CARTESIAN_POINT('Ctrl Pts',(-15.1776335706624,4.32882767782522,251.038960290898));
#14464=CARTESIAN_POINT('Ctrl Pts',(-15.3648739637955,5.38057044757596,250.991777332594));
#14465=CARTESIAN_POINT('Ctrl Pts',(-15.3658371696729,6.43197914685562,250.944594374291));
#14466=CARTESIAN_POINT('Origin',(-6.5,6.43177298256785,260.886209595194));
#14467=CARTESIAN_POINT('',(-15.3655097454245,6.43192356724116,248.077824816097));
#14468=CARTESIAN_POINT('',(-15.3653398059476,6.43183049307641,248.444594374291));
#14469=CARTESIAN_POINT('',(-15.366,6.43177298256785,260.886209595194));
#14470=CARTESIAN_POINT('Ctrl Pts',(-15.3655097454245,6.43192356724116,248.077824816097));
#14471=CARTESIAN_POINT('Ctrl Pts',(-15.3649315115624,5.51512897749327,248.118962474811));
#14472=CARTESIAN_POINT('Ctrl Pts',(-15.2233361525865,4.59815980571514,248.160100133526));
#14473=CARTESIAN_POINT('Ctrl Pts',(-14.94362213897,3.72545982623404,248.20123779224));
#14474=CARTESIAN_POINT('Ctrl Pts',(-14.5016532447144,2.34652911067504,248.266238345123));
#14475=CARTESIAN_POINT('Ctrl Pts',(-13.7148525584771,1.07812238587667,248.331238898007));
#14476=CARTESIAN_POINT('Ctrl Pts',(-12.6758349667039,0.0695447410792356,
248.39623945089));
#14477=CARTESIAN_POINT('Ctrl Pts',(-11.6368173749308,-0.939032903718183,
248.461240003773));
#14478=CARTESIAN_POINT('Ctrl Pts',(-10.3455828776218,-1.68778146851468,
248.526240556656));
#14479=CARTESIAN_POINT('Ctrl Pts',(-8.95412363807302,-2.08856520903101,
248.59124110954));
#14480=CARTESIAN_POINT('Ctrl Pts',(-7.56266439852423,-2.48934894954734,
248.656241662423));
#14481=CARTESIAN_POINT('Ctrl Pts',(-6.07098041673563,-2.54216786578351,
248.721242215306));
#14482=CARTESIAN_POINT('Ctrl Pts',(-4.6546589114767,-2.24080460416003,248.786242768189));
#14483=CARTESIAN_POINT('Ctrl Pts',(-3.23833740621773,-1.93944134253654,
248.851243321073));
#14484=CARTESIAN_POINT('Ctrl Pts',(-1.89737837748844,-1.28389590305338,
248.916243873956));
#14485=CARTESIAN_POINT('Ctrl Pts',(-0.789627099316419,-0.351333021761874,
248.981244426839));
#14486=CARTESIAN_POINT('Ctrl Pts',(0.318124178855573,0.581229859529608,
249.046244979723));
#14487=CARTESIAN_POINT('Ctrl Pts',(1.19266770647031,1.79081018262943,249.111245532606));
#14488=CARTESIAN_POINT('Ctrl Pts',(1.7310603214858,3.13502735775253,249.176246085489));
#14489=CARTESIAN_POINT('Ctrl Pts',(2.26945293650129,4.47924453287563,249.241246638372));
#14490=CARTESIAN_POINT('Ctrl Pts',(2.47169463891752,5.95809856002202,249.306247191256));
#14491=CARTESIAN_POINT('Ctrl Pts',(2.31397940911453,7.39751244355334,249.371247744139));
#14492=CARTESIAN_POINT('Ctrl Pts',(2.15626417931155,8.83692632708468,249.436248297022));
#14493=CARTESIAN_POINT('Ctrl Pts',(1.63859201728934,10.236900067001,249.501248849905));
#14494=CARTESIAN_POINT('Ctrl Pts',(0.821898494138215,11.4326417243236,249.566249402789));
#14495=CARTESIAN_POINT('Ctrl Pts',(0.00520497098708925,12.6283833816463,
249.631249955672));
#14496=CARTESIAN_POINT('Ctrl Pts',(-1.11050991329295,13.6198929563754,249.696250508555));
#14497=CARTESIAN_POINT('Ctrl Pts',(-2.3939145387706,14.290459126946,249.761251061438));
#14498=CARTESIAN_POINT('Ctrl Pts',(-3.67731916424824,14.9610252975167,249.826251614322));
#14499=CARTESIAN_POINT('Ctrl Pts',(-5.12841353092349,15.3106480639289,249.891252167205));
#14500=CARTESIAN_POINT('Ctrl Pts',(-6.5763882532227,15.2981730731075,249.956252720088));
#14501=CARTESIAN_POINT('Ctrl Pts',(-8.02436297552191,15.2856980822862,250.021253272971));
#14502=CARTESIAN_POINT('Ctrl Pts',(-9.46921805344508,14.9111253342314,250.086253825855));
#14503=CARTESIAN_POINT('Ctrl Pts',(-10.7408785326919,14.2185460627152,250.151254378738));
#14504=CARTESIAN_POINT('Ctrl Pts',(-12.0125390119386,13.5259667911989,250.216254931621));
#14505=CARTESIAN_POINT('Ctrl Pts',(-13.111004892509,12.5153809962213,250.281255484505));
#14506=CARTESIAN_POINT('Ctrl Pts',(-13.9069749473838,11.3057454752666,250.346256037388));
#14507=CARTESIAN_POINT('Ctrl Pts',(-14.7029450022585,10.0961099543118,250.411256590271));
#14508=CARTESIAN_POINT('Ctrl Pts',(-15.1964192314376,8.68742470738009,250.476257143154));
#14509=CARTESIAN_POINT('Ctrl Pts',(-15.3293104203217,7.24550711135407,250.541257696038));
#14510=CARTESIAN_POINT('Ctrl Pts',(-15.3542304548097,6.97511569922655,250.553446736057));
#14511=CARTESIAN_POINT('Ctrl Pts',(-15.366470753608,6.70355568692715,250.565635776077));
#14512=CARTESIAN_POINT('Ctrl Pts',(-15.3662080510474,6.43197208529678,250.577824816097));
#14513=CARTESIAN_POINT('Ctrl Pts',(-15.3658371696729,6.43197914685562,250.944594374291));
#14514=CARTESIAN_POINT('Ctrl Pts',(-15.3662009029452,6.82902025267945,250.926776779711));
#14515=CARTESIAN_POINT('Ctrl Pts',(-15.3400010025069,7.22601371914519,250.908959185132));
#14516=CARTESIAN_POINT('Ctrl Pts',(-15.2868376708262,7.61936292802496,250.891141590552));
#14517=CARTESIAN_POINT('Ctrl Pts',(-15.0928919652502,9.05434428532636,250.826141037669));
#14518=CARTESIAN_POINT('Ctrl Pts',(-14.5400977776192,10.4408252759206,250.761140484786));
#14519=CARTESIAN_POINT('Ctrl Pts',(-13.6935249184878,11.6156022022756,250.696139931903));
#14520=CARTESIAN_POINT('Ctrl Pts',(-12.8469520593564,12.7903791286305,250.631139379019));
#14521=CARTESIAN_POINT('Ctrl Pts',(-11.7066005287246,13.7534519907462,250.566138826136));
#14522=CARTESIAN_POINT('Ctrl Pts',(-10.4067019442981,14.391456773424,250.501138273253));
#14523=CARTESIAN_POINT('Ctrl Pts',(-9.10680335987154,15.0294615561018,250.43613772037));
#14524=CARTESIAN_POINT('Ctrl Pts',(-7.64735772165025,15.3423982593419,250.371137167486));
#14525=CARTESIAN_POINT('Ctrl Pts',(-6.20015744952368,15.2934308735567,250.306136614603));
#14526=CARTESIAN_POINT('Ctrl Pts',(-4.75295717739709,15.2444634877715,250.24113606172));
#14527=CARTESIAN_POINT('Ctrl Pts',(-3.3180022713652,14.833592012961,250.176135508837));
#14528=CARTESIAN_POINT('Ctrl Pts',(-2.06420232921192,14.1091804327317,250.111134955953));
#14529=CARTESIAN_POINT('Ctrl Pts',(-0.810402387058642,13.3847688525024,
250.04613440307));
#14530=CARTESIAN_POINT('Ctrl Pts',(0.262242591216055,12.3468171668541,249.981133850187));
#14531=CARTESIAN_POINT('Ctrl Pts',(1.02747077600075,11.1175034323969,249.916133297303));
#14532=CARTESIAN_POINT('Ctrl Pts',(1.79269896078545,9.88818969793975,249.85113274442));
#14533=CARTESIAN_POINT('Ctrl Pts',(2.25051035208017,8.46751391467371,249.786132191537));
#14534=CARTESIAN_POINT('Ctrl Pts',(2.34701563417244,7.0227048743358,249.721131638654));
#14535=CARTESIAN_POINT('Ctrl Pts',(2.44352091626472,5.57789583399789,249.65613108577));
#14536=CARTESIAN_POINT('Ctrl Pts',(2.17872008915453,4.10895353658814,249.591130532887));
#14537=CARTESIAN_POINT('Ctrl Pts',(1.58378305303297,2.78878826073631,249.526129980004));
#14538=CARTESIAN_POINT('Ctrl Pts',(0.988846016911408,1.46862298488449,249.461129427121));
#14539=CARTESIAN_POINT('Ctrl Pts',(0.0637727717784695,0.29723473059058,
249.396128874237));
#14540=CARTESIAN_POINT('Ctrl Pts',(-1.08254563004082,-0.587491528861413,
249.331128321354));
#14541=CARTESIAN_POINT('Ctrl Pts',(-2.22886403186013,-1.47221778831342,
249.266127768471));
#14542=CARTESIAN_POINT('Ctrl Pts',(-3.59642759036579,-2.0702820529235,249.201127215588));
#14543=CARTESIAN_POINT('Ctrl Pts',(-5.02425939287671,-2.31128573806799,
249.136126662704));
#14544=CARTESIAN_POINT('Ctrl Pts',(-6.45209119538764,-2.55228942321248,
249.071126109821));
#14545=CARTESIAN_POINT('Ctrl Pts',(-7.94019124190381,-2.43623252889138,
249.006125556938));
#14546=CARTESIAN_POINT('Ctrl Pts',(-9.31339418105008,-1.97677619752506,
248.941125004055));
#14547=CARTESIAN_POINT('Ctrl Pts',(-10.6865971201963,-1.51731986615874,
248.876124451171));
#14548=CARTESIAN_POINT('Ctrl Pts',(-11.9449029519726,-0.714464097747203,
248.811123898288));
#14549=CARTESIAN_POINT('Ctrl Pts',(-12.9401955711036,0.33728636449107,248.746123345405));
#14550=CARTESIAN_POINT('Ctrl Pts',(-13.9354881902347,1.38903682672936,248.681122792522));
#14551=CARTESIAN_POINT('Ctrl Pts',(-14.6677675967203,2.68968198279439,248.616122239638));
#14552=CARTESIAN_POINT('Ctrl Pts',(-15.0508366428241,4.08612193439743,248.551121686755));
#14553=CARTESIAN_POINT('Ctrl Pts',(-15.2601031498491,4.84898208693241,248.5156125826));
#14554=CARTESIAN_POINT('Ctrl Pts',(-15.3651541248176,5.64043046799048,248.480103478445));
#14555=CARTESIAN_POINT('Ctrl Pts',(-15.3653398059476,6.43183049307641,248.444594374291));
#14556=CARTESIAN_POINT('Origin',(-6.5,6.43177298256785,260.886209595194));
#14557=CARTESIAN_POINT('',(-15.3653307732302,6.43170986456378,245.577824816097));
#14558=CARTESIAN_POINT('',(-15.3655110343894,6.43162198763813,245.944594374291));
#14559=CARTESIAN_POINT('',(-15.366,6.43177298256785,260.886209595194));
#14560=CARTESIAN_POINT('Ctrl Pts',(-15.3653307732302,6.43170986456378,245.577824816097));
#14561=CARTESIAN_POINT('Ctrl Pts',(-15.365491947844,5.77504272427858,245.607288620662));
#14562=CARTESIAN_POINT('Ctrl Pts',(-15.293456027428,5.1184079823648,245.636752425228));
#14563=CARTESIAN_POINT('Ctrl Pts',(-15.1488419680877,4.47816742424782,245.666216229793));
#14564=CARTESIAN_POINT('Ctrl Pts',(-14.8298066652648,3.06572287169104,245.731216782676));
#14565=CARTESIAN_POINT('Ctrl Pts',(-14.1575375418244,1.73306791231306,245.796217335559));
#14566=CARTESIAN_POINT('Ctrl Pts',(-13.2111975505435,0.637061396213097,
245.861217888443));
#14567=CARTESIAN_POINT('Ctrl Pts',(-12.2648575592627,-0.458945119886869,
245.926218441326));
#14568=CARTESIAN_POINT('Ctrl Pts',(-11.0444467001413,-1.31830319270885,
245.991218994209));
#14569=CARTESIAN_POINT('Ctrl Pts',(-9.69360663159018,-1.83985231435453,
246.056219547092));
#14570=CARTESIAN_POINT('Ctrl Pts',(-8.34276656303907,-2.36140143600022,
246.121220099976));
#14571=CARTESIAN_POINT('Ctrl Pts',(-6.86149728505829,-2.54514160646962,
246.186220652859));
#14572=CARTESIAN_POINT('Ctrl Pts',(-5.42416640013887,-2.36944666273369,
246.251221205742));
#14573=CARTESIAN_POINT('Ctrl Pts',(-3.98683551521946,-2.19375171899776,
246.316221758626));
#14574=CARTESIAN_POINT('Ctrl Pts',(-2.59344302336147,-1.65862166105649,
246.381222311509));
#14575=CARTESIAN_POINT('Ctrl Pts',(-1.40800326731247,-0.827046055025128,
246.446222864392));
#14576=CARTESIAN_POINT('Ctrl Pts',(-0.222563511263459,0.00452955100623695,
246.511223417275));
#14577=CARTESIAN_POINT('Ctrl Pts',(0.754923508976573,1.13255070512771,246.576223970159));
#14578=CARTESIAN_POINT('Ctrl Pts',(1.40939574037707,2.4242367681619,246.641224523042));
#14579=CARTESIAN_POINT('Ctrl Pts',(2.06386797177757,3.71592283119607,246.706225075925));
#14580=CARTESIAN_POINT('Ctrl Pts',(2.39532541433854,5.17127380314298,246.771225628808));
#14581=CARTESIAN_POINT('Ctrl Pts',(2.36475258440544,6.6189794563542,246.836226181692));
#14582=CARTESIAN_POINT('Ctrl Pts',(2.33417975447233,8.06668510956546,246.901226734575));
#14583=CARTESIAN_POINT('Ctrl Pts',(1.94157665204511,9.50674544404105,246.966227287458));
#14584=CARTESIAN_POINT('Ctrl Pts',(1.23315659414109,10.7696498045689,247.031227840341));
#14585=CARTESIAN_POINT('Ctrl Pts',(0.524736536237075,12.0325541650966,247.096228393225));
#14586=CARTESIAN_POINT('Ctrl Pts',(-0.499500477143713,13.1183025516767,
247.161228946108));
#14587=CARTESIAN_POINT('Ctrl Pts',(-1.71899062328603,13.8990907662661,247.226229498991));
#14588=CARTESIAN_POINT('Ctrl Pts',(-2.93848076942834,14.6798789808555,247.291230051874));
#14589=CARTESIAN_POINT('Ctrl Pts',(-4.35322404833216,15.1557070234544,247.356230604758));
#14590=CARTESIAN_POINT('Ctrl Pts',(-5.79669004762257,15.2705648051858,247.421231157641));
#14591=CARTESIAN_POINT('Ctrl Pts',(-7.240156046913,15.3854225869173,247.486231710524));
#14592=CARTESIAN_POINT('Ctrl Pts',(-8.71234476659003,15.1393101077814,247.551232263407));
#14593=CARTESIAN_POINT('Ctrl Pts',(-10.0399637617057,14.5611974579483,247.616232816291));
#14594=CARTESIAN_POINT('Ctrl Pts',(-11.3675827568214,13.9830848081152,247.681233369174));
#14595=CARTESIAN_POINT('Ctrl Pts',(-12.5506320273757,13.072971987585,247.746233922057));
#14596=CARTESIAN_POINT('Ctrl Pts',(-13.4498539859601,11.9379890418828,247.811234474941));
#14597=CARTESIAN_POINT('Ctrl Pts',(-14.3490759445444,10.8030060961806,247.876235027824));
#14598=CARTESIAN_POINT('Ctrl Pts',(-14.9644705911588,9.44315302530647,247.941235580707));
#14599=CARTESIAN_POINT('Ctrl Pts',(-15.223599363329,8.01849913670959,248.00623613359));
#14600=CARTESIAN_POINT('Ctrl Pts',(-15.3187302844077,7.49548258588289,248.030099027759));
#14601=CARTESIAN_POINT('Ctrl Pts',(-15.3658451639653,6.96373244877257,248.053961921928));
#14602=CARTESIAN_POINT('Ctrl Pts',(-15.3655097454245,6.43192356724116,248.077824816097));
#14603=CARTESIAN_POINT('Ctrl Pts',(-15.3653398059476,6.43183049307641,248.444594374291));
#14604=CARTESIAN_POINT('Ctrl Pts',(-15.3654940200753,7.08911357072862,248.415102925562));
#14605=CARTESIAN_POINT('Ctrl Pts',(-15.2933138879128,7.74636329323055,248.385611476834));
#14606=CARTESIAN_POINT('Ctrl Pts',(-15.1484271692047,8.38717412578271,248.356120028105));
#14607=CARTESIAN_POINT('Ctrl Pts',(-14.8290899637598,9.79955161842378,248.291119475222));
#14608=CARTESIAN_POINT('Ctrl Pts',(-14.1565568671482,11.1320718565649,248.226118922339));
#14609=CARTESIAN_POINT('Ctrl Pts',(-13.2099922449493,12.2278829025747,248.161118369455));
#14610=CARTESIAN_POINT('Ctrl Pts',(-12.2634276227504,13.3236939485845,248.096117816572));
#14611=CARTESIAN_POINT('Ctrl Pts',(-11.0428314749641,14.182795802463,248.031117263689));
#14612=CARTESIAN_POINT('Ctrl Pts',(-9.69188107233505,14.7040629528314,247.966116710806));
#14613=CARTESIAN_POINT('Ctrl Pts',(-8.34093066970603,15.2253301031998,247.901116157922));
#14614=CARTESIAN_POINT('Ctrl Pts',(-6.8596260122343,15.4087625500582,247.836115605039));
#14615=CARTESIAN_POINT('Ctrl Pts',(-5.42233256080435,15.2327683252499,247.771115052156));
#14616=CARTESIAN_POINT('Ctrl Pts',(-3.98503910937443,15.0567741004416,247.706114499273));
#14617=CARTESIAN_POINT('Ctrl Pts',(-2.5917568639863,14.5213532039666,247.641113946389));
#14618=CARTESIAN_POINT('Ctrl Pts',(-1.40649010340869,13.6895304232192,247.576113393506));
#14619=CARTESIAN_POINT('Ctrl Pts',(-0.221223342831083,12.8577076424717,
247.511112840623));
#14620=CARTESIAN_POINT('Ctrl Pts',(0.756027932935998,11.7294829774518,247.44611228774));
#14621=CARTESIAN_POINT('Ctrl Pts',(1.41023075834464,10.4376605841909,247.381111734856));
#14622=CARTESIAN_POINT('Ctrl Pts',(2.06443358375329,9.14583819092992,247.316111181973));
#14623=CARTESIAN_POINT('Ctrl Pts',(2.3955879588035,7.69041806942788,247.25111062909));
#14624=CARTESIAN_POINT('Ctrl Pts',(2.36471345584747,6.24271879173646,247.186110076207));
#14625=CARTESIAN_POINT('Ctrl Pts',(2.33383895289144,4.79501951404503,247.121109523323));
#14626=CARTESIAN_POINT('Ctrl Pts',(1.94093557192917,3.35504108016422,247.05610897044));
#14627=CARTESIAN_POINT('Ctrl Pts',(1.23225226447099,2.09228441387053,246.991108417557));
#14628=CARTESIAN_POINT('Ctrl Pts',(0.523568957012813,0.829527747576842,
246.926107864673));
#14629=CARTESIAN_POINT('Ctrl Pts',(-0.500894276941281,-0.256007151129717,
246.86110731179));
#14630=CARTESIAN_POINT('Ctrl Pts',(-1.7205471282046,-1.03654117677531,246.796106758907));
#14631=CARTESIAN_POINT('Ctrl Pts',(-2.94019997946792,-1.81707520242089,
246.731106206024));
#14632=CARTESIAN_POINT('Ctrl Pts',(-4.35504244804047,-2.29260835500551,
246.66610565314));
#14633=CARTESIAN_POINT('Ctrl Pts',(-5.79853236018863,-2.40716526386096,
246.601105100257));
#14634=CARTESIAN_POINT('Ctrl Pts',(-7.24202227233679,-2.5217221727164,246.536104547374));
#14635=CARTESIAN_POINT('Ctrl Pts',(-8.71415962806057,-2.27530283784268,
246.471103994491));
#14636=CARTESIAN_POINT('Ctrl Pts',(-10.0416581120634,-1.69691348952389,
246.406103441607));
#14637=CARTESIAN_POINT('Ctrl Pts',(-11.3691565960662,-1.11852414120512,
246.341102888724));
#14638=CARTESIAN_POINT('Ctrl Pts',(-12.552016208348,-0.208164779441313,
246.276102335841));
#14639=CARTESIAN_POINT('Ctrl Pts',(-13.4510015518931,0.927005588855917,
246.211101782958));
#14640=CARTESIAN_POINT('Ctrl Pts',(-14.3499868954382,2.06217595715318,246.146101230074));
#14641=CARTESIAN_POINT('Ctrl Pts',(-14.9650979702466,3.42215733198388,246.081100677191));
#14642=CARTESIAN_POINT('Ctrl Pts',(-15.2239298637372,4.84686516798998,246.016100124308));
#14643=CARTESIAN_POINT('Ctrl Pts',(-15.3188417162853,5.36929560819389,245.992264874302));
#14644=CARTESIAN_POINT('Ctrl Pts',(-15.365846922726,5.90042941315193,245.968429624296));
#14645=CARTESIAN_POINT('Ctrl Pts',(-15.3655110343894,6.43162198763813,245.944594374291));
#14646=CARTESIAN_POINT('Origin',(-6.5,6.43177298256785,263.507698758713));
#14647=CARTESIAN_POINT('',(-13.9450882934309,6.43189944074375,247.257698758713));
#14648=CARTESIAN_POINT('',(-13.9450893758793,6.43164617986677,246.764720431675));
#14649=CARTESIAN_POINT('',(-13.9455,6.43177298256789,263.507698758713));
#14650=CARTESIAN_POINT('',(-13.5606802741685,4.06871967504022,244.886209595194));
#14651=CARTESIAN_POINT('Ctrl Pts',(-13.9450882934309,6.43189944074375,247.257698758713));
#14652=CARTESIAN_POINT('Ctrl Pts',(-13.9453699716111,6.8785025342968,247.233835864544));
#14653=CARTESIAN_POINT('Ctrl Pts',(-13.7980287498298,8.54143185980366,247.144972417492));
#14654=CARTESIAN_POINT('Ctrl Pts',(-12.5747094635392,11.2446313388274,246.991108417557));
#14655=CARTESIAN_POINT('Ctrl Pts',(-9.59420190300037,13.5375182117999,246.796106758907));
#14656=CARTESIAN_POINT('Ctrl Pts',(-5.88525273346894,14.1575601010644,246.601105100257));
#14657=CARTESIAN_POINT('Ctrl Pts',(-2.3210283651816,12.9587857864344,246.406103441607));
#14658=CARTESIAN_POINT('Ctrl Pts',(0.259376558051009,10.2234125812861,246.211101782958));
#14659=CARTESIAN_POINT('Ctrl Pts',(1.24847865565592,6.59540585209445,246.016100124308));
#14660=CARTESIAN_POINT('Ctrl Pts',(0.413423482436507,2.92887675386613,245.821098465658));
#14661=CARTESIAN_POINT('Ctrl Pts',(-2.04920214666245,0.0870039240630693,
245.626096807008));
#14662=CARTESIAN_POINT('Ctrl Pts',(-5.55963654711201,-1.26117254099502,
245.431095148358));
#14663=CARTESIAN_POINT('Ctrl Pts',(-9.29146276272433,-0.798267925870965,
245.236093489709));
#14664=CARTESIAN_POINT('Ctrl Pts',(-12.1552397329513,1.21827415889713,245.054464971987));
#14665=CARTESIAN_POINT('Ctrl Pts',(-13.2531691625695,3.15293886147087,244.937837007149));
#14666=CARTESIAN_POINT('Ctrl Pts',(-13.5606802741685,4.06871967504022,244.886209595194));
#14667=CARTESIAN_POINT('',(-6.56569596473014,-1.01343717499105,244.886209595194));
#14668=CARTESIAN_POINT('Origin',(-6.5,6.43177298256785,244.886209595194));
#14669=CARTESIAN_POINT('Ctrl Pts',(-13.9450893758793,6.43164617986677,246.764720431674));
#14670=CARTESIAN_POINT('Ctrl Pts',(-13.9446022147054,7.20207006749424,246.723555128797));
#14671=CARTESIAN_POINT('Ctrl Pts',(-13.6375150380194,9.18938303346644,246.617389273036));
#14672=CARTESIAN_POINT('Ctrl Pts',(-11.8969968350143,11.9939777077968,246.446222864392));
#14673=CARTESIAN_POINT('Ctrl Pts',(-8.64354351795149,13.8796529333669,246.251221205742));
#14674=CARTESIAN_POINT('Ctrl Pts',(-4.88544464111068,14.0119423198044,246.056219547092));
#14675=CARTESIAN_POINT('Ctrl Pts',(-1.50746712882826,12.3596870112171,245.861217888443));
#14676=CARTESIAN_POINT('Ctrl Pts',(0.695205395144706,9.31189841214496,245.666216229793));
#14677=CARTESIAN_POINT('Ctrl Pts',(1.20387608653361,5.58602334650667,245.471214571143));
#14678=CARTESIAN_POINT('Ctrl Pts',(-0.100899992062858,2.05939046574996,
245.276212912493));
#14679=CARTESIAN_POINT('Ctrl Pts',(-2.91261395215861,-0.438036016167426,
245.081211253844));
#14680=CARTESIAN_POINT('Ctrl Pts',(-5.34941510741743,-1.02416954420736,
244.951210148077));
#14681=CARTESIAN_POINT('Ctrl Pts',(-6.56569596473014,-1.01343717499105,
244.886209595194));
#14682=CARTESIAN_POINT('Origin',(-6.5,6.43177298256785,263.507698758713));
#14683=CARTESIAN_POINT('',(-13.9456747173555,6.43194018529407,249.757698758713));
#14684=CARTESIAN_POINT('',(-13.9449455814553,6.43182127881114,249.264720431674));
#14685=CARTESIAN_POINT('',(-13.9455,6.43177298256789,263.507698758713));
#14686=CARTESIAN_POINT('Ctrl Pts',(-13.9456747173555,6.43194018529407,249.757698758713));
#14687=CARTESIAN_POINT('Ctrl Pts',(-13.9458953300235,6.66001098452012,249.745509718693));
#14688=CARTESIAN_POINT('Ctrl Pts',(-13.8808003634927,8.10419059181383,249.66832012579));
#14689=CARTESIAN_POINT('Ctrl Pts',(-12.9742685135307,10.6920016007892,249.526129980004));
#14690=CARTESIAN_POINT('Ctrl Pts',(-10.2068555718026,13.2380144148563,249.331128321354));
#14691=CARTESIAN_POINT('Ctrl Pts',(-6.56676923658599,14.1816918552946,249.136126662704));
#14692=CARTESIAN_POINT('Ctrl Pts',(-2.91096398943488,13.3008719904214,248.941125004055));
#14693=CARTESIAN_POINT('Ctrl Pts',(-0.100094881300308,10.8029187289803,
248.746123345405));
#14694=CARTESIAN_POINT('Ctrl Pts',(1.20409914610878,7.27590390362059,248.551121686755));
#14695=CARTESIAN_POINT('Ctrl Pts',(0.69458281563053,3.55016253464298,248.356120028105));
#14696=CARTESIAN_POINT('Ctrl Pts',(-1.50869278831339,0.502814137742552,
248.161118369455));
#14697=CARTESIAN_POINT('Ctrl Pts',(-4.88702928111861,-1.14873004328783,
247.966116710806));
#14698=CARTESIAN_POINT('Ctrl Pts',(-8.64509371369493,-1.0156610468397,247.771115052156));
#14699=CARTESIAN_POINT('Ctrl Pts',(-11.898157028509,0.870693827689635,247.576113393506));
#14700=CARTESIAN_POINT('Ctrl Pts',(-13.6378083554075,3.67519753547724,247.404974629025));
#14701=CARTESIAN_POINT('Ctrl Pts',(-13.9446027035121,5.66199259233763,247.298836417427));
#14702=CARTESIAN_POINT('Ctrl Pts',(-13.9450882934309,6.43189944074375,247.257698758713));
#14703=CARTESIAN_POINT('Ctrl Pts',(-13.9449455814553,6.43182127881113,249.264720431674));
#14704=CARTESIAN_POINT('Ctrl Pts',(-13.9450750875784,6.9837952416646,249.235228982946));
#14705=CARTESIAN_POINT('Ctrl Pts',(-13.7508600937365,8.75225627081592,249.140736981334));
#14706=CARTESIAN_POINT('Ctrl Pts',(-12.3650517689522,11.4980209748333,248.981244426839));
#14707=CARTESIAN_POINT('Ctrl Pts',(-9.28995072507354,13.6623936974992,248.78624276819));
#14708=CARTESIAN_POINT('Ctrl Pts',(-5.55803537636869,14.1245230511257,248.59124110954));
#14709=CARTESIAN_POINT('Ctrl Pts',(-2.0478787246529,12.7756138638807,248.39623945089));
#14710=CARTESIAN_POINT('Ctrl Pts',(0.414152983126427,9.93322832020636,248.20123779224));
#14711=CARTESIAN_POINT('Ctrl Pts',(1.24844462516442,6.26652501049171,248.006236133591));
#14712=CARTESIAN_POINT('Ctrl Pts',(0.258586022766082,2.63872461703594,247.811234474941));
#14713=CARTESIAN_POINT('Ctrl Pts',(-2.32238882781091,-0.0961107388132638,
247.616232816291));
#14714=CARTESIAN_POINT('Ctrl Pts',(-5.88686308895128,-1.29414212418505,
247.421231157641));
#14715=CARTESIAN_POINT('Ctrl Pts',(-9.59568285503789,-0.673327159893731,
247.226229498991));
#14716=CARTESIAN_POINT('Ctrl Pts',(-12.5757126012294,1.62018083514774,247.031227840341));
#14717=CARTESIAN_POINT('Ctrl Pts',(-13.7982484981895,4.32314964520486,246.877391484569));
#14718=CARTESIAN_POINT('Ctrl Pts',(-13.9453714485852,5.98556064937529,246.78855568168));
#14719=CARTESIAN_POINT('Ctrl Pts',(-13.9450893758793,6.43164617986677,246.764720431674));
#14720=CARTESIAN_POINT('Origin',(-6.5,6.43177298256785,263.507698758713));
#14721=CARTESIAN_POINT('',(-13.9461111697801,6.43178251580015,252.257698758713));
#14722=CARTESIAN_POINT('',(-13.9453632581547,6.4319461154582,251.764720431675));
#14723=CARTESIAN_POINT('',(-13.9455,6.43177298256789,263.507698758713));
#14724=CARTESIAN_POINT('Ctrl Pts',(-13.9461111697801,6.43178251580015,252.257698758713));
#14725=CARTESIAN_POINT('Ctrl Pts',(-13.9461119198476,6.44142059139145,252.257183572842));
#14726=CARTESIAN_POINT('Ctrl Pts',(-13.9437802412465,7.66708591080191,252.191667834088));
#14727=CARTESIAN_POINT('Ctrl Pts',(-13.3237017886373,10.1063878691313,252.061151542451));
#14728=CARTESIAN_POINT('Ctrl Pts',(-10.7908096390754,12.8858146082488,251.866149883801));
#14729=CARTESIAN_POINT('Ctrl Pts',(-7.24776877019554,14.1458213704849,251.671148225152));
#14730=CARTESIAN_POINT('Ctrl Pts',(-3.52868707706655,13.5897755097268,251.476146566502));
#14731=CARTESIAN_POINT('Ctrl Pts',(-0.509116244652642,11.3485821607565,
251.281144907852));
#14732=CARTESIAN_POINT('Ctrl Pts',(1.10007191826787,7.94986635978842,251.086143249202));
#14733=CARTESIAN_POINT('Ctrl Pts',(0.920039966399679,4.19375878202392,250.891141590553));
#14734=CARTESIAN_POINT('Ctrl Pts',(-1.00682871322467,0.964527800673052,
250.696139931903));
#14735=CARTESIAN_POINT('Ctrl Pts',(-4.22690786058867,-0.977596274700365,
250.501138273253));
#14736=CARTESIAN_POINT('Ctrl Pts',(-7.98212170435301,-1.1753957363637,250.306136614603));
#14737=CARTESIAN_POINT('Ctrl Pts',(-11.388412275481,0.417695656017143,250.111134955953));
#14738=CARTESIAN_POINT('Ctrl Pts',(-13.5028831869044,3.23854942376843,249.928322337323));
#14739=CARTESIAN_POINT('Ctrl Pts',(-13.9447188677778,5.44377672635221,249.810510271577));
#14740=CARTESIAN_POINT('Ctrl Pts',(-13.9456747173555,6.43194018529407,249.757698758713));
#14741=CARTESIAN_POINT('Ctrl Pts',(-13.9453632581547,6.4319461154582,251.764720431675));
#14742=CARTESIAN_POINT('Ctrl Pts',(-13.9456687145137,6.76537376641815,251.746902837095));
#14743=CARTESIAN_POINT('Ctrl Pts',(-13.8434001356862,8.31499635810809,251.664084689632));
#14744=CARTESIAN_POINT('Ctrl Pts',(-12.7876966929006,10.9628403258599,251.516265989286));
#14745=CARTESIAN_POINT('Ctrl Pts',(-9.91475940844803,13.3891517385202,251.321264330637));
#14746=CARTESIAN_POINT('Ctrl Pts',(-6.23791443911237,14.1775468064111,251.126262671987));
#14747=CARTESIAN_POINT('Ctrl Pts',(-2.62277003818962,13.142420402497,250.931261013337));
#14748=CARTESIAN_POINT('Ctrl Pts',(0.0795911796349016,10.5274635080144,
250.736259354687));
#14749=CARTESIAN_POINT('Ctrl Pts',(1.23297535983508,6.94829312306938,250.541257696038));
#14750=CARTESIAN_POINT('Ctrl Pts',(0.565851101460774,3.24752280656896,250.346256037388));
#14751=CARTESIAN_POINT('Ctrl Pts',(-1.76472622088437,0.29639335224502,250.151254378738));
#14752=CARTESIAN_POINT('Ctrl Pts',(-5.21008866443971,-1.21033600106685,
249.956252720088));
#14753=CARTESIAN_POINT('Ctrl Pts',(-8.95912393276911,-0.91794881180413,
249.761251061438));
#14754=CARTESIAN_POINT('Ctrl Pts',(-12.1292286261452,1.10472069768431,249.566249402789));
#14755=CARTESIAN_POINT('Ctrl Pts',(-13.6950805877014,3.88592381615938,249.400739192867));
#14756=CARTESIAN_POINT('Ctrl Pts',(-13.9447896499357,5.76721842670446,249.300229535829));
#14757=CARTESIAN_POINT('Ctrl Pts',(-13.9449455814553,6.43182127881113,249.264720431674));
#14758=CARTESIAN_POINT('Origin',(-6.5,6.43177298256785,263.507698758713));
#14759=CARTESIAN_POINT('',(-13.9457314253814,6.43161246431689,254.757698758713));
#14760=CARTESIAN_POINT('',(-13.9459749743085,6.43187801484696,254.264720431675));
#14761=CARTESIAN_POINT('',(-13.9455,6.43177298256789,263.507698758713));
#14762=CARTESIAN_POINT('Ctrl Pts',(-13.9457314253814,6.43161246431689,254.757698758713));
#14763=CARTESIAN_POINT('Ctrl Pts',(-13.9447764467647,7.43903318707587,254.703856874108));
#14764=CARTESIAN_POINT('Ctrl Pts',(-13.4899053046119,9.66349788843306,254.58501443662));
#14765=CARTESIAN_POINT('Ctrl Pts',(-11.3415429435809,12.4836456341042,254.401171446249));
#14766=CARTESIAN_POINT('Ctrl Pts',(-7.92297884889648,14.0502263597522,254.206169787599));
#14767=CARTESIAN_POINT('Ctrl Pts',(-4.16941497964704,13.8232595805219,254.011168128949));
#14768=CARTESIAN_POINT('Ctrl Pts',(-0.964520865428091,11.8561781495442,
253.816166470299));
#14769=CARTESIAN_POINT('Ctrl Pts',(0.937202605263502,8.61207527194551,253.62116481165));
#14770=CARTESIAN_POINT('Ctrl Pts',(1.088048894503,4.85468242098349,253.426163153));
#14771=CARTESIAN_POINT('Ctrl Pts',(-0.547494453099542,1.46857055077819,
253.23116149435));
#14772=CARTESIAN_POINT('Ctrl Pts',(-3.58438541588777,-0.749096899397535,
253.0361598357));
#14773=CARTESIAN_POINT('Ctrl Pts',(-7.3076746545037,-1.27623339504218,252.84115817705));
#14774=CARTESIAN_POINT('Ctrl Pts',(-10.8408199374328,0.0112603133497307,
252.646156518401));
#14775=CARTESIAN_POINT('Ctrl Pts',(-13.3454084612837,2.80288567302779,252.451670045622));
#14776=CARTESIAN_POINT('Ctrl Pts',(-13.9460172844921,5.22539298308426,252.322184125726));
#14777=CARTESIAN_POINT('Ctrl Pts',(-13.9461111697801,6.43178251580015,252.257698758713));
#14778=CARTESIAN_POINT('Ctrl Pts',(-13.9459749743085,6.43187801484696,254.264720431675));
#14779=CARTESIAN_POINT('Ctrl Pts',(-13.9460556454763,6.54682096936603,254.258576691244));
#14780=CARTESIAN_POINT('Ctrl Pts',(-13.9158492372516,7.87781383709142,254.187432397931));
#14781=CARTESIAN_POINT('Ctrl Pts',(-13.1616603427751,10.3925787653421,254.051287551734));
#14782=CARTESIAN_POINT('Ctrl Pts',(-10.5131299782381,13.0620436217747,253.856285893084));
#14783=CARTESIAN_POINT('Ctrl Pts',(-6.91982264875327,14.1706004076339,253.661284234434));
#14784=CARTESIAN_POINT('Ctrl Pts',(-3.2276800535143,13.4572710531101,253.466282575784));
#14785=CARTESIAN_POINT('Ctrl Pts',(-0.305911835418159,11.0899886045361,
253.271280917135));
#14786=CARTESIAN_POINT('Ctrl Pts',(1.15763503213971,7.62606217949973,253.076279258485));
#14787=CARTESIAN_POINT('Ctrl Pts',(0.818410191934892,3.88097443428047,252.881277599835));
#14788=CARTESIAN_POINT('Ctrl Pts',(-1.24372554496956,0.736399436894482,
252.686275941185));
#14789=CARTESIAN_POINT('Ctrl Pts',(-4.54330114888175,-1.06736233941388,
252.491274282535));
#14790=CARTESIAN_POINT('Ctrl Pts',(-8.30352567567975,-1.10566664296319,
252.296272623886));
#14791=CARTESIAN_POINT('Ctrl Pts',(-11.6391615339537,0.630504181754365,
252.101270965236));
#14792=CARTESIAN_POINT('Ctrl Pts',(-13.5706939065415,3.44899169520534,251.924086901166));
#14793=CARTESIAN_POINT('Ctrl Pts',(-13.9445543759801,5.54899287042243,251.811903389978));
#14794=CARTESIAN_POINT('Ctrl Pts',(-13.9453632581547,6.4319461154582,251.764720431675));
#14795=CARTESIAN_POINT('Origin',(-6.5,6.43177298256785,263.507698758713));
#14796=CARTESIAN_POINT('',(-13.9451274702829,6.4316349637354,257.257698758713));
#14797=CARTESIAN_POINT('',(-13.9459987791106,6.43167704459545,256.764720431675));
#14798=CARTESIAN_POINT('',(-13.9455,6.43177298256789,263.507698758713));
#14799=CARTESIAN_POINT('Ctrl Pts',(-13.9451274702829,6.4316349637354,257.257698758713));
#14800=CARTESIAN_POINT('Ctrl Pts',(-13.9445812522303,7.22081373064257,257.215530728257));
#14801=CARTESIAN_POINT('Ctrl Pts',(-13.6267827690106,9.22691426686787,257.108362144918));
#14802=CARTESIAN_POINT('Ctrl Pts',(-11.8547914355129,12.034620997221,256.936193008696));
#14803=CARTESIAN_POINT('Ctrl Pts',(-8.58717183770218,13.8956470450103,256.741191350046));
#14804=CARTESIAN_POINT('Ctrl Pts',(-4.82818696338679,13.9995164531848,256.546189691396));
#14805=CARTESIAN_POINT('Ctrl Pts',(-1.46278287172395,12.3217767520604,256.351188032747));
#14806=CARTESIAN_POINT('Ctrl Pts',(0.716752195883785,9.25740360642712,256.156186374097));
#14807=CARTESIAN_POINT('Ctrl Pts',(1.19730882121199,5.52781638254676,255.961184715447));
#14808=CARTESIAN_POINT('Ctrl Pts',(-0.134246313555596,2.01103993266644,
255.766183056797));
#14809=CARTESIAN_POINT('Ctrl Pts',(-2.96443655298958,-0.465001028602228,
255.571181398147));
#14810=CARTESIAN_POINT('Ctrl Pts',(-6.62697433982785,-1.31739330731701,
255.376179739498));
#14811=CARTESIAN_POINT('Ctrl Pts',(-10.2596196416587,-0.345465453031489,
255.181178080848));
#14812=CARTESIAN_POINT('Ctrl Pts',(-13.0071697546051,2.22196984587269,254.986176422198));
#14813=CARTESIAN_POINT('Ctrl Pts',(-13.8871469687636,4.79794250018219,254.845016648153));
#14814=CARTESIAN_POINT('Ctrl Pts',(-13.9459293435947,6.22282568531489,254.768857426991));
#14815=CARTESIAN_POINT('Ctrl Pts',(-13.9457314253814,6.43161246431689,254.757698758713));
#14816=CARTESIAN_POINT('Ctrl Pts',(-13.9459987791106,6.43167704459545,256.764720431675));
#14817=CARTESIAN_POINT('Ctrl Pts',(-13.9452724247665,7.54429640133474,256.70524999251));
#14818=CARTESIAN_POINT('Ctrl Pts',(-13.4158824236672,9.87366517330999,256.580779000462));
#14819=CARTESIAN_POINT('Ctrl Pts',(-11.0804296656676,12.6836019176416,256.391307455531));
#14820=CARTESIAN_POINT('Ctrl Pts',(-7.59848046310273,14.1037376364226,256.196305796881));
#14821=CARTESIAN_POINT('Ctrl Pts',(-3.85792537225687,13.7177281451327,256.001304138232));
#14822=CARTESIAN_POINT('Ctrl Pts',(-0.739371378738949,11.616448368688,255.806302479582));
#14823=CARTESIAN_POINT('Ctrl Pts',(1.02300694803562,8.29458468304415,255.611300820932));
#14824=CARTESIAN_POINT('Ctrl Pts',(1.01430790860051,4.53417512584038,255.416299162282));
#14825=CARTESIAN_POINT('Ctrl Pts',(-0.763420556208652,1.22050084837849,
255.221297503632));
#14826=CARTESIAN_POINT('Ctrl Pts',(-3.89166299529113,-0.866328074636114,
255.026295844983));
#14827=CARTESIAN_POINT('Ctrl Pts',(-7.63396397027625,-1.23502730735099,
254.831294186333));
#14828=CARTESIAN_POINT('Ctrl Pts',(-11.1093054787138,0.201202866177523,
254.636292527683));
#14829=CARTESIAN_POINT('Ctrl Pts',(-13.4242112656194,3.01277957123129,254.447434609464));
#14830=CARTESIAN_POINT('Ctrl Pts',(-13.9452021474203,5.33072864278933,254.323577244128));
#14831=CARTESIAN_POINT('Ctrl Pts',(-13.9459749743085,6.43187801484696,254.264720431675));
#14832=CARTESIAN_POINT('Ctrl Pts',(-9.81139348551471,-0.236820829780501,
259.706335652578));
#14833=CARTESIAN_POINT('Ctrl Pts',(-10.9008030290343,0.304142342813418,
259.641335099694));
#14834=CARTESIAN_POINT('Ctrl Pts',(-12.8083812201165,1.9297800108904,259.511333993928));
#14835=CARTESIAN_POINT('Ctrl Pts',(-14.1851462695771,5.42940748028812,259.316332335278));
#14836=CARTESIAN_POINT('Ctrl Pts',(-13.7523257580445,9.16467808570731,259.121330676628));
#14837=CARTESIAN_POINT('Ctrl Pts',(-11.6122793516618,12.2567796777562,258.926329017979));
#14838=CARTESIAN_POINT('Ctrl Pts',(-8.26862653170071,13.9774677413128,258.731327359329));
#14839=CARTESIAN_POINT('Ctrl Pts',(-4.50862938937823,13.9217796100182,258.536325700679));
#14840=CARTESIAN_POINT('Ctrl Pts',(-1.21743004662297,12.1027648942659,258.341324042029));
#14841=CARTESIAN_POINT('Ctrl Pts',(0.830132802421682,8.94868564322478,258.146322383379));
#14842=CARTESIAN_POINT('Ctrl Pts',(1.15202784967473,5.20206719240598,257.951320724729));
#14843=CARTESIAN_POINT('Ctrl Pts',(-0.327530058757188,1.74494971672666,
257.75631906608));
#14844=CARTESIAN_POINT('Ctrl Pts',(-3.26021932302907,-0.608789762765702,
257.56131740743));
#14845=CARTESIAN_POINT('Ctrl Pts',(-6.95562279721707,-1.30502921472525,
257.36631574878));
#14846=CARTESIAN_POINT('Ctrl Pts',(-10.5437627550554,-0.179859485232368,
257.17131409013));
#14847=CARTESIAN_POINT('Ctrl Pts',(-13.1799141928899,2.50183057058523,256.976312431481));
#14848=CARTESIAN_POINT('Ctrl Pts',(-14.2434703748362,6.10871341464289,256.781310772831));
#14849=CARTESIAN_POINT('Ctrl Pts',(-13.4840473786807,9.79165143481236,256.586309114181));
#14850=CARTESIAN_POINT('Ctrl Pts',(-11.0804296656676,12.6836019176416,256.391307455531));
#14851=CARTESIAN_POINT('Ctrl Pts',(-7.59848046310273,14.1037376364226,256.196305796881));
#14852=CARTESIAN_POINT('Ctrl Pts',(-3.85792537225687,13.7177281451327,256.001304138232));
#14853=CARTESIAN_POINT('Ctrl Pts',(-0.739371378738949,11.616448368688,255.806302479582));
#14854=CARTESIAN_POINT('Ctrl Pts',(1.02300694803562,8.29458468304415,255.611300820932));
#14855=CARTESIAN_POINT('Ctrl Pts',(1.01430790860051,4.53417512584038,255.416299162282));
#14856=CARTESIAN_POINT('Ctrl Pts',(-0.763420556208652,1.22050084837849,
255.221297503632));
#14857=CARTESIAN_POINT('Ctrl Pts',(-3.89166299529113,-0.866328074636114,
255.026295844983));
#14858=CARTESIAN_POINT('Ctrl Pts',(-7.63396397027625,-1.23502730735099,
254.831294186333));
#14859=CARTESIAN_POINT('Ctrl Pts',(-11.1093054787138,0.201202866177523,
254.636292527683));
#14860=CARTESIAN_POINT('Ctrl Pts',(-13.4995175085847,3.10424302502025,254.441290869033));
#14861=CARTESIAN_POINT('Ctrl Pts',(-14.2418928265339,6.79065518305518,254.246289210384));
#14862=CARTESIAN_POINT('Ctrl Pts',(-13.1616603427751,10.3925787653421,254.051287551734));
#14863=CARTESIAN_POINT('Ctrl Pts',(-10.5131299782381,13.0620436217747,253.856285893084));
#14864=CARTESIAN_POINT('Ctrl Pts',(-6.91982264875327,14.1706004076339,253.661284234434));
#14865=CARTESIAN_POINT('Ctrl Pts',(-3.2276800535143,13.4572710531101,253.466282575784));
#14866=CARTESIAN_POINT('Ctrl Pts',(-0.305911835418159,11.0899886045361,
253.271280917135));
#14867=CARTESIAN_POINT('Ctrl Pts',(1.15763503213971,7.62606217949973,253.076279258485));
#14868=CARTESIAN_POINT('Ctrl Pts',(0.818410191934892,3.88097443428047,252.881277599835));
#14869=CARTESIAN_POINT('Ctrl Pts',(-1.24372554496956,0.736399436894482,
252.686275941185));
#14870=CARTESIAN_POINT('Ctrl Pts',(-4.54330114888175,-1.06736233941388,
252.491274282535));
#14871=CARTESIAN_POINT('Ctrl Pts',(-8.30352567567975,-1.10566664296319,
252.296272623886));
#14872=CARTESIAN_POINT('Ctrl Pts',(-11.6391615339537,0.630504181754365,
252.101270965236));
#14873=CARTESIAN_POINT('Ctrl Pts',(-13.7649284214359,3.73241824434344,251.906269306586));
#14874=CARTESIAN_POINT('Ctrl Pts',(-14.1803751693297,7.46981837160677,251.711267647936));
#14875=CARTESIAN_POINT('Ctrl Pts',(-12.7876966929006,10.9628403258599,251.516265989286));
#14876=CARTESIAN_POINT('Ctrl Pts',(-9.91475940844803,13.3891517385202,251.321264330637));
#14877=CARTESIAN_POINT('Ctrl Pts',(-6.23791443911237,14.1775468064111,251.126262671987));
#14878=CARTESIAN_POINT('Ctrl Pts',(-2.62277003818962,13.142420402497,250.931261013337));
#14879=CARTESIAN_POINT('Ctrl Pts',(0.0795911796349016,10.5274635080144,
250.736259354687));
#14880=CARTESIAN_POINT('Ctrl Pts',(1.23297535983508,6.94829312306938,250.541257696038));
#14881=CARTESIAN_POINT('Ctrl Pts',(0.565851101460774,3.24752280656896,250.346256037388));
#14882=CARTESIAN_POINT('Ctrl Pts',(-1.76472622088437,0.29639335224502,250.151254378738));
#14883=CARTESIAN_POINT('Ctrl Pts',(-5.21008866443971,-1.21033600106685,
249.956252720088));
#14884=CARTESIAN_POINT('Ctrl Pts',(-8.95912393276911,-0.91794881180413,
249.761251061438));
#14885=CARTESIAN_POINT('Ctrl Pts',(-12.1292286261452,1.10472069768431,249.566249402789));
#14886=CARTESIAN_POINT('Ctrl Pts',(-13.974092032751,4.38149269502769,249.371247744139));
#14887=CARTESIAN_POINT('Ctrl Pts',(-14.0593936945629,8.14094469474752,249.176246085489));
#14888=CARTESIAN_POINT('Ctrl Pts',(-12.3650517689522,11.4980209748333,248.981244426839));
#14889=CARTESIAN_POINT('Ctrl Pts',(-9.28995072507354,13.6623936974992,248.78624276819));
#14890=CARTESIAN_POINT('Ctrl Pts',(-5.55803537636869,14.1245230511257,248.59124110954));
#14891=CARTESIAN_POINT('Ctrl Pts',(-2.0478787246529,12.7756138638807,248.39623945089));
#14892=CARTESIAN_POINT('Ctrl Pts',(0.414152983126427,9.93322832020636,248.20123779224));
#14893=CARTESIAN_POINT('Ctrl Pts',(1.24844462516442,6.26652501049171,248.006236133591));
#14894=CARTESIAN_POINT('Ctrl Pts',(0.258586022766082,2.63872461703594,247.811234474941));
#14895=CARTESIAN_POINT('Ctrl Pts',(-2.32238882781091,-0.0961107388132638,
247.616232816291));
#14896=CARTESIAN_POINT('Ctrl Pts',(-5.88686308895128,-1.29414212418505,
247.421231157641));
#14897=CARTESIAN_POINT('Ctrl Pts',(-9.59568285503789,-0.673327159893731,
247.226229498991));
#14898=CARTESIAN_POINT('Ctrl Pts',(-12.5757126012294,1.62018083514774,247.031227840341));
#14899=CARTESIAN_POINT('Ctrl Pts',(-14.1253887260271,5.04644115309334,246.836226181692));
#14900=CARTESIAN_POINT('Ctrl Pts',(-13.8798855290331,8.79883785724345,246.641224523042));
#14901=CARTESIAN_POINT('Ctrl Pts',(-11.8969968350143,11.9939777077968,246.446222864392));
#14902=CARTESIAN_POINT('Ctrl Pts',(-8.64354351795149,13.8796529333669,246.251221205742));
#14903=CARTESIAN_POINT('Ctrl Pts',(-4.88544464111068,14.0119423198044,246.056219547092));
#14904=CARTESIAN_POINT('Ctrl Pts',(-1.50746712882826,12.3596870112171,245.861217888443));
#14905=CARTESIAN_POINT('Ctrl Pts',(0.695205395144706,9.31189841214496,245.666216229793));
#14906=CARTESIAN_POINT('Ctrl Pts',(1.20387608653361,5.58602334650667,245.471214571143));
#14907=CARTESIAN_POINT('Ctrl Pts',(-0.100899992062858,2.05939046574996,
245.276212912493));
#14908=CARTESIAN_POINT('Ctrl Pts',(-2.91261395215861,-0.438036016167426,
245.081211253844));
#14909=CARTESIAN_POINT('Ctrl Pts',(-5.34941510741743,-1.02416954420736,
244.951210148077));
#14910=CARTESIAN_POINT('Ctrl Pts',(-6.56569596473014,-1.01343717499105,
244.886209595194));
#14911=CARTESIAN_POINT('Ctrl Pts',(-10.02198307861,-0.66091312313178,259.432960300116));
#14912=CARTESIAN_POINT('Ctrl Pts',(-11.1806741235541,-0.0855471485469646,
259.367959747233));
#14913=CARTESIAN_POINT('Ctrl Pts',(-13.2095656278426,1.64347369538583,259.237958641467));
#14914=CARTESIAN_POINT('Ctrl Pts',(-14.6738866844109,5.36566158473652,259.042956982817));
#14915=CARTESIAN_POINT('Ctrl Pts',(-14.2135407532006,9.33847844382113,258.847955324167));
#14916=CARTESIAN_POINT('Ctrl Pts',(-11.9373971104438,12.6272236600504,258.652953665517));
#14917=CARTESIAN_POINT('Ctrl Pts',(-8.38110315016291,14.4573396731194,258.457952006867));
#14918=CARTESIAN_POINT('Ctrl Pts',(-4.38198725867788,14.3981100294794,258.262950348218));
#14919=CARTESIAN_POINT('Ctrl Pts',(-0.881482578632365,12.4634142355041,
258.067948689568));
#14920=CARTESIAN_POINT('Ctrl Pts',(1.29629597238295,9.10874986252786,257.872947030918));
#14921=CARTESIAN_POINT('Ctrl Pts',(1.63866208334889,5.12386348659151,257.677945372268));
#14922=CARTESIAN_POINT('Ctrl Pts',(0.0650110086229034,1.44688903357902,
257.482943713618));
#14923=CARTESIAN_POINT('Ctrl Pts',(-3.0541839794597,-1.05653759164428,257.287942054969));
#14924=CARTESIAN_POINT('Ctrl Pts',(-6.98459833874984,-1.79705471206167,
257.092940396319));
#14925=CARTESIAN_POINT('Ctrl Pts',(-10.8009277089898,-0.600329295655229,
256.897938737669));
#14926=CARTESIAN_POINT('Ctrl Pts',(-13.604726411053,2.25190407376516,256.702937079019));
#14927=CARTESIAN_POINT('Ctrl Pts',(-14.7359199379931,6.08816829270179,256.50793542037));
#14928=CARTESIAN_POINT('Ctrl Pts',(-13.9282010868005,10.0053244516867,256.31293376172));
#14929=CARTESIAN_POINT('Ctrl Pts',(-11.3717241988344,13.0811898567669,256.11793210307));
#14930=CARTESIAN_POINT('Ctrl Pts',(-7.66833883383393,14.5916397603364,255.92293044442));
#14931=CARTESIAN_POINT('Ctrl Pts',(-3.68990142003924,14.1810818177503,255.72792878577));
#14932=CARTESIAN_POINT('Ctrl Pts',(-0.373021549692262,11.9461701866086,
255.532927127121));
#14933=CARTESIAN_POINT('Ctrl Pts',(1.50143603807589,8.41305105067232,255.337925468471));
#14934=CARTESIAN_POINT('Ctrl Pts',(1.49218377922334,4.41349651659178,255.142923809821));
#14935=CARTESIAN_POINT('Ctrl Pts',(-0.398600145674072,0.889087598020738,
254.947922151171));
#14936=CARTESIAN_POINT('Ctrl Pts',(-3.72578460274132,-1.33045417101461,
254.752920492521));
#14937=CARTESIAN_POINT('Ctrl Pts',(-7.70607893098081,-1.7226010011629,254.557918833872));
#14938=CARTESIAN_POINT('Ctrl Pts',(-11.4024363825041,-0.195033108587213,
254.362917175222));
#14939=CARTESIAN_POINT('Ctrl Pts',(-13.9446550467372,2.89262722555766,254.167915516572));
#14940=CARTESIAN_POINT('Ctrl Pts',(-14.7342420647803,6.81347846180485,253.972913857922));
#14941=CARTESIAN_POINT('Ctrl Pts',(-13.5853116989371,10.6444680324354,253.777912199273));
#14942=CARTESIAN_POINT('Ctrl Pts',(-10.7683468266292,13.4836987352882,253.582910540623));
#14943=CARTESIAN_POINT('Ctrl Pts',(-6.94652146336407,14.6627547002629,253.387908881973));
#14944=CARTESIAN_POINT('Ctrl Pts',(-3.01957536012084,13.9040608370604,253.192907223323));
#14945=CARTESIAN_POINT('Ctrl Pts',(0.0880040528270217,11.3862299714022,
252.997905564673));
#14946=CARTESIAN_POINT('Ctrl Pts',(1.64462585716397,7.70201355076388,252.802903906023));
#14947=CARTESIAN_POINT('Ctrl Pts',(1.28382785708581,3.71875522635433,252.607902247374));
#14948=CARTESIAN_POINT('Ctrl Pts',(-0.909450351301318,0.374199534419655,
252.412900588724));
#14949=CARTESIAN_POINT('Ctrl Pts',(-4.41886398468801,-1.54427330240607,
252.217898930074));
#14950=CARTESIAN_POINT('Ctrl Pts',(-8.41822172126895,-1.5850135857728,252.022897271424));
#14951=CARTESIAN_POINT('Ctrl Pts',(-11.9659888774937,0.261569821780531,
251.827895612775));
#14952=CARTESIAN_POINT('Ctrl Pts',(-14.2269448887718,3.56075153713113,251.632893954125));
#14953=CARTESIAN_POINT('Ctrl Pts',(-14.6688121638469,7.53583334598187,251.437892295475));
#14954=CARTESIAN_POINT('Ctrl Pts',(-13.1875656585965,11.2509956394116,251.242890636825));
#14955=CARTESIAN_POINT('Ctrl Pts',(-10.1319226049963,13.8316094433007,251.047888978176));
#14956=CARTESIAN_POINT('Ctrl Pts',(-6.2212469872179,14.6701428584681,250.852887319526));
#14957=CARTESIAN_POINT('Ctrl Pts',(-2.37619581390419,13.5691871143815,250.657885660876));
#14958=CARTESIAN_POINT('Ctrl Pts',(0.498023309586833,10.7879308324116,250.462884002226));
#14959=CARTESIAN_POINT('Ctrl Pts',(1.72475748768169,6.98114145918213,250.267882343576));
#14960=CARTESIAN_POINT('Ctrl Pts',(1.01520715498863,3.04501895077211,250.072880684927));
#14961=CARTESIAN_POINT('Ctrl Pts',(-1.46358430504108,-0.0937889397377692,
249.877879026277));
#14962=CARTESIAN_POINT('Ctrl Pts',(-5.12805615925029,-1.69633943988909,
249.682877367627));
#14963=CARTESIAN_POINT('Ctrl Pts',(-9.1155130513194,-1.38535775272618,249.487875708977));
#14964=CARTESIAN_POINT('Ctrl Pts',(-12.4872220120131,0.765944355344317,
249.292874050327));
#14965=CARTESIAN_POINT('Ctrl Pts',(-14.449410356236,4.25110417630493,249.097872391678));
#14966=CARTESIAN_POINT('Ctrl Pts',(-14.5401368164991,8.24964025659253,248.902870733028));
#14967=CARTESIAN_POINT('Ctrl Pts',(-12.7380424361471,11.8202113481242,248.707869074378));
#14968=CARTESIAN_POINT('Ctrl Pts',(-9.46737892577495,14.1222283504466,248.512867415728));
#14969=CARTESIAN_POINT('Ctrl Pts',(-5.49813070249999,14.613747033056,248.317865757078));
#14970=CARTESIAN_POINT('Ctrl Pts',(-1.76474402263465,13.1790533450843,248.122864098429));
#14971=CARTESIAN_POINT('Ctrl Pts',(0.853861724985316,10.1559049842816,247.927862439779));
#14972=CARTESIAN_POINT('Ctrl Pts',(1.74121052806084,6.25601598963642,247.732860781129));
#14973=CARTESIAN_POINT('Ctrl Pts',(0.688401412166355,2.39750396011843,247.537859122479));
#14974=CARTESIAN_POINT('Ctrl Pts',(-2.0567117221724,-0.511254509154269,
247.34285746383));
#14975=CARTESIAN_POINT('Ctrl Pts',(-5.84787036483852,-1.78547525198674,
247.14785580518));
#14976=CARTESIAN_POINT('Ctrl Pts',(-9.79255423128669,-1.12517927425215,
246.95285414653));
#14977=CARTESIAN_POINT('Ctrl Pts',(-12.9621003410296,1.31418541753933,246.75785248788));
#14978=CARTESIAN_POINT('Ctrl Pts',(-14.6103288323697,4.95834033766709,246.56285082923));
#14979=CARTESIAN_POINT('Ctrl Pts',(-14.3492127465467,8.94937243761533,246.367849170581));
#14980=CARTESIAN_POINT('Ctrl Pts',(-12.2402213332185,12.3477086778318,246.172847511931));
#14981=CARTESIAN_POINT('Ctrl Pts',(-8.77986315474553,14.3533042874336,245.977845853281));
#14982=CARTESIAN_POINT('Ctrl Pts',(-4.78276624980934,14.4940066783003,245.782844194631));
#14983=CARTESIAN_POINT('Ctrl Pts',(-1.18996470259768,12.7366754327557,245.587842535981));
#14984=CARTESIAN_POINT('Ctrl Pts',(1.15278779452702,9.49506131469077,245.392840877332));
#14985=CARTESIAN_POINT('Ctrl Pts',(1.6938076326989,5.5322375090646,245.197839218682));
#14986=CARTESIAN_POINT('Ctrl Pts',(0.306053718736717,1.78132678678773,245.002837560032));
#14987=CARTESIAN_POINT('Ctrl Pts',(-2.68447248501027,-0.874924681925421,
244.807835901382));
#14988=CARTESIAN_POINT('Ctrl Pts',(-5.27624313150744,-1.49833364150479,
244.677834795616));
#14989=CARTESIAN_POINT('Ctrl Pts',(-6.56987392984997,-1.48691874232758,
244.612834242732));
#14990=CARTESIAN_POINT('Ctrl Pts',(-10.2325726717054,-1.08500541648306,
259.159584947655));
#14991=CARTESIAN_POINT('Ctrl Pts',(-11.460545218074,-0.475236639907348,
259.094584394772));
#14992=CARTESIAN_POINT('Ctrl Pts',(-13.6107500355688,1.35716737988126,258.964583289005));
#14993=CARTESIAN_POINT('Ctrl Pts',(-15.1626270992447,5.30191568918491,258.769581630356));
#14994=CARTESIAN_POINT('Ctrl Pts',(-14.6747557483566,9.51227880193497,258.574579971706));
#14995=CARTESIAN_POINT('Ctrl Pts',(-12.2625148692259,12.9976676423447,258.379578313056));
#14996=CARTESIAN_POINT('Ctrl Pts',(-8.49357976862511,14.9372116049259,258.184576654406));
#14997=CARTESIAN_POINT('Ctrl Pts',(-4.25534512797754,14.8744404489405,257.989574995756));
#14998=CARTESIAN_POINT('Ctrl Pts',(-0.545535110641766,12.8240635767423,
257.794573337107));
#14999=CARTESIAN_POINT('Ctrl Pts',(1.76245914234423,9.26881408183094,257.599571678457));
#15000=CARTESIAN_POINT('Ctrl Pts',(2.12529631702305,5.04565978077704,257.404570019807));
#15001=CARTESIAN_POINT('Ctrl Pts',(0.457552076003,1.14882835043138,257.209568361157));
#15002=CARTESIAN_POINT('Ctrl Pts',(-2.84814863589033,-1.50428542052285,
257.014566702508));
#15003=CARTESIAN_POINT('Ctrl Pts',(-7.01357388028262,-2.28908020939808,
256.819565043858));
#15004=CARTESIAN_POINT('Ctrl Pts',(-11.0580926629242,-1.02079910607809,
256.624563385208));
#15005=CARTESIAN_POINT('Ctrl Pts',(-14.0295386292161,2.0019775769451,256.429561726558));
#15006=CARTESIAN_POINT('Ctrl Pts',(-15.22836950115,6.06762317076068,256.234560067908));
#15007=CARTESIAN_POINT('Ctrl Pts',(-14.3723547949202,10.218997468561,256.039558409258));
#15008=CARTESIAN_POINT('Ctrl Pts',(-11.6630187320013,13.4787777958922,255.844556750609));
#15009=CARTESIAN_POINT('Ctrl Pts',(-7.73819720456513,15.0795418842502,255.649555091959));
#15010=CARTESIAN_POINT('Ctrl Pts',(-3.52187746782161,14.644435490368,255.454553433309));
#15011=CARTESIAN_POINT('Ctrl Pts',(-0.00667172064557749,12.2758920045292,
255.259551774659));
#15012=CARTESIAN_POINT('Ctrl Pts',(1.97986512811616,8.53151741830049,255.06455011601));
#15013=CARTESIAN_POINT('Ctrl Pts',(1.97005964984618,4.29281790734318,254.86954845736));
#15014=CARTESIAN_POINT('Ctrl Pts',(-0.0337797351394938,0.557674347662983,
254.67454679871));
#15015=CARTESIAN_POINT('Ctrl Pts',(-3.5599062101915,-1.7945802673931,254.47954514006));
#15016=CARTESIAN_POINT('Ctrl Pts',(-7.77819389168537,-2.21017469497481,
254.28454348141));
#15017=CARTESIAN_POINT('Ctrl Pts',(-11.6955672862944,-0.591269083351945,
254.089541822761));
#15018=CARTESIAN_POINT('Ctrl Pts',(-14.3897925848898,2.68101142609504,253.894540164111));
#15019=CARTESIAN_POINT('Ctrl Pts',(-15.2265913030267,6.83630174055454,253.699538505461));
#15020=CARTESIAN_POINT('Ctrl Pts',(-14.0089630550991,10.8963572995288,253.504536846811));
#15021=CARTESIAN_POINT('Ctrl Pts',(-11.0235636750202,13.9053538488017,253.309535188162));
#15022=CARTESIAN_POINT('Ctrl Pts',(-6.97322027797486,15.1549089928918,253.114533529512));
#15023=CARTESIAN_POINT('Ctrl Pts',(-2.81147066672739,14.3508506210107,252.919531870862));
#15024=CARTESIAN_POINT('Ctrl Pts',(0.481919941072204,11.6824713382684,252.724530212212));
#15025=CARTESIAN_POINT('Ctrl Pts',(2.13161668218823,7.77796492202803,252.529528553562));
#15026=CARTESIAN_POINT('Ctrl Pts',(1.74924552223673,3.55653601842819,252.334526894913));
#15027=CARTESIAN_POINT('Ctrl Pts',(-0.575175157633071,0.0119996319448261,
252.139525236263));
#15028=CARTESIAN_POINT('Ctrl Pts',(-4.29442682049427,-2.02118426539827,
251.944523577613));
#15029=CARTESIAN_POINT('Ctrl Pts',(-8.53291776685814,-2.0643605285824,251.749521918963));
#15030=CARTESIAN_POINT('Ctrl Pts',(-12.2928162210337,-0.107364538193309,
251.554520260313));
#15031=CARTESIAN_POINT('Ctrl Pts',(-14.6889613561078,3.38908482991881,251.359518601664));
#15032=CARTESIAN_POINT('Ctrl Pts',(-15.1572491583641,7.601848320357,251.164516943014));
#15033=CARTESIAN_POINT('Ctrl Pts',(-13.5874346242923,11.5391509529632,250.969515284364));
#15034=CARTESIAN_POINT('Ctrl Pts',(-10.3490858015446,14.2740671480813,250.774513625714));
#15035=CARTESIAN_POINT('Ctrl Pts',(-6.20457953532343,15.162738910525,250.579511967064));
#15036=CARTESIAN_POINT('Ctrl Pts',(-2.12962158961875,13.9959538262661,250.384510308415));
#15037=CARTESIAN_POINT('Ctrl Pts',(0.916455439538768,11.0483981568087,250.189508649765));
#15038=CARTESIAN_POINT('Ctrl Pts',(2.2165396155283,7.01398979529488,249.994506991115));
#15039=CARTESIAN_POINT('Ctrl Pts',(1.46456320851649,2.84251509497526,249.799505332465));
#15040=CARTESIAN_POINT('Ctrl Pts',(-1.16244238919778,-0.483971231720556,
249.604503673815));
#15041=CARTESIAN_POINT('Ctrl Pts',(-5.04602365406088,-2.18234287871134,
249.409502015166));
#15042=CARTESIAN_POINT('Ctrl Pts',(-9.27190216986969,-1.85276669364823,
249.214500356516));
#15043=CARTESIAN_POINT('Ctrl Pts',(-12.845215397881,0.427168013004334,249.019498697866));
#15044=CARTESIAN_POINT('Ctrl Pts',(-14.924728679721,4.12071565758218,248.824497039216));
#15045=CARTESIAN_POINT('Ctrl Pts',(-15.0208799384352,8.35833581843755,248.629495380566));
#15046=CARTESIAN_POINT('Ctrl Pts',(-13.1110331033419,12.1424017214152,248.434493721917));
#15047=CARTESIAN_POINT('Ctrl Pts',(-9.64480712647635,14.582063003394,248.239492063267));
#15048=CARTESIAN_POINT('Ctrl Pts',(-5.43822602863129,15.1029710149863,248.044490404617));
#15049=CARTESIAN_POINT('Ctrl Pts',(-1.48160932061641,13.5824928262879,247.849488745967));
#15050=CARTESIAN_POINT('Ctrl Pts',(1.2935704668442,10.3785816483567,247.654487087318));
#15051=CARTESIAN_POINT('Ctrl Pts',(2.23397643095727,6.24550696878113,247.459485428668));
#15052=CARTESIAN_POINT('Ctrl Pts',(1.11821680156663,2.15628330320092,247.264483770018));
#15053=CARTESIAN_POINT('Ctrl Pts',(-1.79103461653389,-0.926398279495272,
247.069482111368));
#15054=CARTESIAN_POINT('Ctrl Pts',(-5.80887764072575,-2.27680837978843,
246.874480452719));
#15055=CARTESIAN_POINT('Ctrl Pts',(-9.98942560753549,-1.57703138861056,
246.679478794069));
#15056=CARTESIAN_POINT('Ctrl Pts',(-13.3484880808298,1.00818999993092,246.484477135419));
#15057=CARTESIAN_POINT('Ctrl Pts',(-15.0952689387123,4.87023952224083,246.289475476769));
#15058=CARTESIAN_POINT('Ctrl Pts',(-14.8185399640602,9.09990701798722,246.094473818119));
#15059=CARTESIAN_POINT('Ctrl Pts',(-12.5834458314227,12.7014396478669,245.899472159469));
#15060=CARTESIAN_POINT('Ctrl Pts',(-8.91618279153957,14.8269556415003,245.70447050082));
#15061=CARTESIAN_POINT('Ctrl Pts',(-4.68008785850801,14.9760710367962,245.50946884217));
#15062=CARTESIAN_POINT('Ctrl Pts',(-0.872462276367092,13.1136638542943,
245.31446718352));
#15063=CARTESIAN_POINT('Ctrl Pts',(1.61037019390933,9.67822421723656,245.11946552487));
#15064=CARTESIAN_POINT('Ctrl Pts',(2.18373917886419,5.47845167162253,244.924463866221));
#15065=CARTESIAN_POINT('Ctrl Pts',(0.713007429536295,1.5032631078255,244.729462207571));
#15066=CARTESIAN_POINT('Ctrl Pts',(-2.45633101786194,-1.31181334768342,
244.534460548921));
#15067=CARTESIAN_POINT('Ctrl Pts',(-5.20307115559744,-1.97249773880223,
244.404459443155));
#15068=CARTESIAN_POINT('Ctrl Pts',(-6.5740518949698,-1.96040030966411,244.339458890271));
#15069=CARTESIAN_POINT('Ctrl Pts',(-10.4431622648007,-1.50909770983434,
258.886209595194));
#15070=CARTESIAN_POINT('Ctrl Pts',(-11.7404163125939,-0.864926131267731,
258.82120904231));
#15071=CARTESIAN_POINT('Ctrl Pts',(-14.011934443295,1.07086106437669,258.691207936544));
#15072=CARTESIAN_POINT('Ctrl Pts',(-15.6513675140784,5.23816979363331,258.496206277894));
#15073=CARTESIAN_POINT('Ctrl Pts',(-15.1359707435126,9.68607916004879,258.301204619244));
#15074=CARTESIAN_POINT('Ctrl Pts',(-12.5876326280079,13.3681116246389,258.106202960595));
#15075=CARTESIAN_POINT('Ctrl Pts',(-8.60605638708732,15.4170835367325,257.911201301945));
#15076=CARTESIAN_POINT('Ctrl Pts',(-4.1287029972772,15.3507708684016,257.716199643295));
#15077=CARTESIAN_POINT('Ctrl Pts',(-0.209587642651167,13.1847129179805,
257.521197984645));
#15078=CARTESIAN_POINT('Ctrl Pts',(2.2286223123055,9.42887830113402,257.326196325996));
#15079=CARTESIAN_POINT('Ctrl Pts',(2.61193055069722,4.96745607496257,257.131194667346));
#15080=CARTESIAN_POINT('Ctrl Pts',(0.850093143383091,0.850767667283733,
256.936193008696));
#15081=CARTESIAN_POINT('Ctrl Pts',(-2.64211329232096,-1.95203324940143,
256.741191350046));
#15082=CARTESIAN_POINT('Ctrl Pts',(-7.04254942181539,-2.7811057067345,256.546189691396));
#15083=CARTESIAN_POINT('Ctrl Pts',(-11.3152576168586,-1.44126891650095,
256.351188032747));
#15084=CARTESIAN_POINT('Ctrl Pts',(-14.4543508473792,1.75205108012504,256.156186374097));
#15085=CARTESIAN_POINT('Ctrl Pts',(-15.720819064307,6.04707804881958,255.961184715447));
#15086=CARTESIAN_POINT('Ctrl Pts',(-14.8165085030399,10.4326704854353,255.766183056797));
#15087=CARTESIAN_POINT('Ctrl Pts',(-11.9543132651681,13.8763657350175,255.571181398147));
#15088=CARTESIAN_POINT('Ctrl Pts',(-7.80805557529633,15.567444008164,255.376179739498));
#15089=CARTESIAN_POINT('Ctrl Pts',(-3.35385351560398,15.1077891629856,255.181178080848));
#15090=CARTESIAN_POINT('Ctrl Pts',(0.359678108401108,12.6056138224498,254.986176422198));
#15091=CARTESIAN_POINT('Ctrl Pts',(2.45829421815644,8.64998378592866,254.791174763548));
#15092=CARTESIAN_POINT('Ctrl Pts',(2.44793552046902,4.17213929809458,254.596173104898));
#15093=CARTESIAN_POINT('Ctrl Pts',(0.331040675395088,0.226261097305232,
254.401171446249));
#15094=CARTESIAN_POINT('Ctrl Pts',(-3.39402781764168,-2.25870636377159,
254.206169787599));
#15095=CARTESIAN_POINT('Ctrl Pts',(-7.85030885238992,-2.69774838878672,
254.011168128949));
#15096=CARTESIAN_POINT('Ctrl Pts',(-11.9886981900848,-0.987505058116681,
253.816166470299));
#15097=CARTESIAN_POINT('Ctrl Pts',(-14.8349301230424,2.46939562663245,253.62116481165));
#15098=CARTESIAN_POINT('Ctrl Pts',(-15.7189405412732,6.85912501930421,253.426163153));
#15099=CARTESIAN_POINT('Ctrl Pts',(-14.432614411261,11.1482465666222,253.23116149435));
#15100=CARTESIAN_POINT('Ctrl Pts',(-11.2787805234113,14.3270089623151,253.0361598357));
#15101=CARTESIAN_POINT('Ctrl Pts',(-6.99991909258566,15.6470632855208,252.84115817705));
#15102=CARTESIAN_POINT('Ctrl Pts',(-2.60336597333394,14.797640404961,252.646156518401));
#15103=CARTESIAN_POINT('Ctrl Pts',(0.875835829317383,11.9787127051345,252.451154859751));
#15104=CARTESIAN_POINT('Ctrl Pts',(2.6186075072125,7.85391629329219,252.256153201101));
#15105=CARTESIAN_POINT('Ctrl Pts',(2.21466318738765,3.39431681050205,252.061151542451));
#15106=CARTESIAN_POINT('Ctrl Pts',(-0.240899963964826,-0.35020027053,251.866149883801));
#15107=CARTESIAN_POINT('Ctrl Pts',(-4.16998965630053,-2.49809522839046,
251.671148225152));
#15108=CARTESIAN_POINT('Ctrl Pts',(-8.64761381244733,-2.54370747139201,
251.476146566502));
#15109=CARTESIAN_POINT('Ctrl Pts',(-12.6196435645737,-0.476298898167143,
251.281144907852));
#15110=CARTESIAN_POINT('Ctrl Pts',(-15.1509778234438,3.2174181227065,251.086143249202));
#15111=CARTESIAN_POINT('Ctrl Pts',(-15.6456861528812,7.66786329473211,250.891141590552));
#15112=CARTESIAN_POINT('Ctrl Pts',(-13.9873035899882,11.8273062665149,250.696139931903));
#15113=CARTESIAN_POINT('Ctrl Pts',(-10.5662489980928,14.7165248528618,250.501138273253));
#15114=CARTESIAN_POINT('Ctrl Pts',(-6.18791208342896,15.6553349625819,250.306136614603));
#15115=CARTESIAN_POINT('Ctrl Pts',(-1.88304736533332,14.4227205381506,250.111134955953));
#15116=CARTESIAN_POINT('Ctrl Pts',(1.3348875694907,11.3088654812059,249.916133297304));
#15117=CARTESIAN_POINT('Ctrl Pts',(2.7083217433749,7.04683813140763,249.721131638654));
#15118=CARTESIAN_POINT('Ctrl Pts',(1.91391926204435,2.6400112391784,249.526129980004));
#15119=CARTESIAN_POINT('Ctrl Pts',(-0.861300473354484,-0.874153523703345,
249.331128321354));
#15120=CARTESIAN_POINT('Ctrl Pts',(-4.96399114887146,-2.66834631753358,
249.136126662704));
#15121=CARTESIAN_POINT('Ctrl Pts',(-9.42829128841997,-2.32017563457029,
248.941125004055));
#15122=CARTESIAN_POINT('Ctrl Pts',(-13.203208783749,0.0883916706643461,
248.746123345405));
#15123=CARTESIAN_POINT('Ctrl Pts',(-15.400047003206,3.99032713885942,248.551121686755));
#15124=CARTESIAN_POINT('Ctrl Pts',(-15.5016230603713,8.46703138028256,248.356120028105));
#15125=CARTESIAN_POINT('Ctrl Pts',(-13.4840237705367,12.4645920947061,248.161118369455));
#15126=CARTESIAN_POINT('Ctrl Pts',(-9.82223532717777,15.0418976563414,247.966116710806));
#15127=CARTESIAN_POINT('Ctrl Pts',(-5.37832135476258,15.5921949969166,247.771115052156));
#15128=CARTESIAN_POINT('Ctrl Pts',(-1.19847461859816,13.9859323074916,247.576113393506));
#15129=CARTESIAN_POINT('Ctrl Pts',(1.73327920870309,10.6012583124319,247.381111734856));
#15130=CARTESIAN_POINT('Ctrl Pts',(2.7267423338537,6.23499794792585,247.186110076207));
#15131=CARTESIAN_POINT('Ctrl Pts',(1.54803219096691,1.9150626462834,246.991108417557));
#15132=CARTESIAN_POINT('Ctrl Pts',(-1.52535751089537,-1.34154204983628,
246.796106758907));
#15133=CARTESIAN_POINT('Ctrl Pts',(-5.76988491661299,-2.76814150759012,
246.601105100257));
#15134=CARTESIAN_POINT('Ctrl Pts',(-10.1862969837843,-2.02888350296897,
246.406103441607));
#15135=CARTESIAN_POINT('Ctrl Pts',(-13.7348758206299,0.702194582322504,
246.211101782958));
#15136=CARTESIAN_POINT('Ctrl Pts',(-15.5802090450549,4.78213870681457,246.016100124308));
#15137=CARTESIAN_POINT('Ctrl Pts',(-15.2878671815738,9.2504415983591,245.821098465658));
#15138=CARTESIAN_POINT('Ctrl Pts',(-12.9266703296268,13.0551706179019,245.626096807008));
#15139=CARTESIAN_POINT('Ctrl Pts',(-9.05250242833362,15.3006069955669,245.431095148358));
#15140=CARTESIAN_POINT('Ctrl Pts',(-4.57740946720667,15.4581353952922,245.236093489709));
#15141=CARTESIAN_POINT('Ctrl Pts',(-0.55495985013651,13.4906522758328,245.041091831059));
#15142=CARTESIAN_POINT('Ctrl Pts',(2.06795259329165,9.86138711978237,244.846090172409));
#15143=CARTESIAN_POINT('Ctrl Pts',(2.67367072502948,5.42466583418046,244.651088513759));
#15144=CARTESIAN_POINT('Ctrl Pts',(1.11996114033587,1.22519942886328,244.456086855109));
#15145=CARTESIAN_POINT('Ctrl Pts',(-2.22818955071361,-1.74870201344141,
244.26108519646));
#15146=CARTESIAN_POINT('Ctrl Pts',(-5.12989917968745,-2.44666183609966,
244.131084090693));
#15147=CARTESIAN_POINT('Ctrl Pts',(-6.57822986008963,-2.43388187700064,
244.06608353781));
#15148=CARTESIAN_POINT('',(1.35783022118007,10.5382254078893,244.886209595194));
#15149=CARTESIAN_POINT('Ctrl Pts',(1.35783022118005,10.5382254078893,244.886209595194));
#15150=CARTESIAN_POINT('Ctrl Pts',(1.44612453701632,10.3322518660377,244.886209595194));
#15151=CARTESIAN_POINT('Ctrl Pts',(1.52645926284569,10.1232070326722,244.886209595194));
#15152=CARTESIAN_POINT('Ctrl Pts',(1.59855524492759,9.91148368960094,244.886209595194));
#15153=CARTESIAN_POINT('Ctrl Pts',(1.62235034055961,9.84160493838024,244.886209595194));
#15154=CARTESIAN_POINT('Ctrl Pts',(1.64524757363912,9.77143430421354,244.886209595194));
#15155=CARTESIAN_POINT('Ctrl Pts',(1.66723568404851,9.70098564097099,244.886209595194));
#15156=CARTESIAN_POINT('Ctrl Pts',(1.73428193209586,9.48617325089184,244.886209595194));
#15157=CARTESIAN_POINT('Ctrl Pts',(1.79287933654356,9.26877589137054,244.886209595194));
#15158=CARTESIAN_POINT('Ctrl Pts',(1.84297302431785,9.04930371074398,244.886209595194));
#15159=CARTESIAN_POINT('Ctrl Pts',(1.87603200511803,8.90446457176506,244.886209595194));
#15160=CARTESIAN_POINT('Ctrl Pts',(1.90538633684054,8.75872169973192,244.886209595194));
#15161=CARTESIAN_POINT('Ctrl Pts',(1.93100783513905,8.61222265349245,244.886209595194));
#15162=CARTESIAN_POINT('Ctrl Pts',(1.94498351169985,8.53231228826498,244.886209595194));
#15163=CARTESIAN_POINT('Ctrl Pts',(1.95784837163251,8.4521769598324,244.886209595194));
#15164=CARTESIAN_POINT('Ctrl Pts',(1.96959660574002,8.37184087900914,244.886209595194));
#15165=CARTESIAN_POINT('Ctrl Pts',(1.9744444460328,8.33869066375004,244.886209595194));
#15166=CARTESIAN_POINT('Ctrl Pts',(1.9791010319949,8.30551366411067,244.886209595194));
#15167=CARTESIAN_POINT('Ctrl Pts',(1.98356526472234,8.27231899002343,244.886209595194));
#15168=CARTESIAN_POINT('Ctrl Pts',(2.01445345584743,8.04264381398712,244.886209595194));
#15169=CARTESIAN_POINT('Ctrl Pts',(2.03615445359886,7.81201163614733,244.886209595194));
#15170=CARTESIAN_POINT('Ctrl Pts',(2.0486294556759,7.58098506779262,244.886209595194));
#15171=CARTESIAN_POINT('Ctrl Pts',(2.06049372757049,7.36126870983855,244.886209595194));
#15172=CARTESIAN_POINT('Ctrl Pts',(2.06401275803726,7.14119496682215,244.886209595194));
#15173=CARTESIAN_POINT('Ctrl Pts',(2.05910149824557,6.92125450421733,244.886209595194));
#15174=CARTESIAN_POINT('Ctrl Pts',(2.05424336876142,6.70369337093213,244.886209595194));
#15175=CARTESIAN_POINT('Ctrl Pts',(2.04113625189595,6.48626204324774,244.886209595194));
#15176=CARTESIAN_POINT('Ctrl Pts',(2.01964971505158,6.269451442371,244.886209595194));
#15177=CARTESIAN_POINT('Ctrl Pts',(2.01639547174321,6.23661439412089,244.886209595194));
#15178=CARTESIAN_POINT('Ctrl Pts',(2.01294892710205,6.20379162458676,244.886209595194));
#15179=CARTESIAN_POINT('Ctrl Pts',(2.00930953270603,6.17098488517774,244.886209595194));
#15180=CARTESIAN_POINT('Ctrl Pts',(2.00630892643853,6.14393639931019,244.886209595194));
#15181=CARTESIAN_POINT('Ctrl Pts',(2.00317717352014,6.11689875710319,244.886209595194));
#15182=CARTESIAN_POINT('Ctrl Pts',(1.99991584422701,6.08988743774954,244.886209595194));
#15183=CARTESIAN_POINT('Ctrl Pts',(1.97636664962037,5.89484585842114,244.886209595194));
#15184=CARTESIAN_POINT('Ctrl Pts',(1.94604394622207,5.7009870739249,244.886209595194));
#15185=CARTESIAN_POINT('Ctrl Pts',(1.90892370423999,5.50865142732287,244.886209595194));
#15186=CARTESIAN_POINT('Ctrl Pts',(1.86788311620583,5.29600281257819,244.886209595194));
#15187=CARTESIAN_POINT('Ctrl Pts',(1.81853400561323,5.08521528319918,244.886209595194));
#15188=CARTESIAN_POINT('Ctrl Pts',(1.76110289217776,4.87672733760996,244.886209595194));
#15189=CARTESIAN_POINT('Ctrl Pts',(1.70358231321742,4.66791461190828,244.886209595194));
#15190=CARTESIAN_POINT('Ctrl Pts',(1.63795418042196,4.46140801599686,244.886209595194));
#15191=CARTESIAN_POINT('Ctrl Pts',(1.56439908283895,4.2576707604985,244.886209595194));
#15192=CARTESIAN_POINT('Ctrl Pts',(1.49132900904767,4.05527695255748,244.886209595194));
#15193=CARTESIAN_POINT('Ctrl Pts',(1.4104357775497,3.85561551861747,244.886209595194));
#15194=CARTESIAN_POINT('Ctrl Pts',(1.32185571267682,3.65917173235668,244.886209595194));
#15195=CARTESIAN_POINT('Ctrl Pts',(1.24882078352789,3.49720235434942,244.886209595194));
#15196=CARTESIAN_POINT('Ctrl Pts',(1.17055942664986,3.33742078495956,244.886209595194));
#15197=CARTESIAN_POINT('Ctrl Pts',(1.08712975796364,3.18011922062368,244.886209595194));
#15198=CARTESIAN_POINT('Ctrl Pts',(1.06774798914291,3.14357607472478,244.886209595194));
#15199=CARTESIAN_POINT('Ctrl Pts',(1.04808722558642,3.10716685946348,244.886209595194));
#15200=CARTESIAN_POINT('Ctrl Pts',(1.02814808042046,3.07089540111588,244.886209595194));
#15201=CARTESIAN_POINT('Ctrl Pts',(1.016081461071,3.0489449174072,244.886209595194));
#15202=CARTESIAN_POINT('Ctrl Pts',(1.00391674600177,3.02705193333218,244.886209595194));
#15203=CARTESIAN_POINT('Ctrl Pts',(0.991656577595838,3.00522125082147,244.886209595194));
#15204=CARTESIAN_POINT('Ctrl Pts',(0.887876283843254,2.82042814123545,244.886209595194));
#15205=CARTESIAN_POINT('Ctrl Pts',(0.7772079883397,2.64000206338419,244.886209595194));
#15206=CARTESIAN_POINT('Ctrl Pts',(0.65985027631292,2.4643596296731,244.886209595194));
#15207=CARTESIAN_POINT('Ctrl Pts',(0.5432329056121,2.28982522158744,244.886209595194));
#15208=CARTESIAN_POINT('Ctrl Pts',(0.420009851735265,2.12001376445838,244.886209595194));
#15209=CARTESIAN_POINT('Ctrl Pts',(0.290335941433409,1.95536608718829,244.886209595194));
#15210=CARTESIAN_POINT('Ctrl Pts',(0.262431134777017,1.91993520066724,244.886209595194));
#15211=CARTESIAN_POINT('Ctrl Pts',(0.234227468440425,1.88474357202413,244.886209595194));
#15212=CARTESIAN_POINT('Ctrl Pts',(0.205726268029875,1.8497958261869,244.886209595194));
#15213=CARTESIAN_POINT('Ctrl Pts',(0.0722508515782293,1.68613026605338,
244.886209595194));
#15214=CARTESIAN_POINT('Ctrl Pts',(-0.067747844306486,1.52781003253958,
244.886209595194));
#15215=CARTESIAN_POINT('Ctrl Pts',(-0.213892779609048,1.3751614069749,244.886209595194));
#15216=CARTESIAN_POINT('Ctrl Pts',(-0.359010861923027,1.2235853310476,244.886209595194));
#15217=CARTESIAN_POINT('Ctrl Pts',(-0.510189741931271,1.07760112169485,
244.886209595194));
#15218=CARTESIAN_POINT('Ctrl Pts',(-0.667082292412142,0.937574313239984,
244.886209595194));
#15219=CARTESIAN_POINT('Ctrl Pts',(-0.74952988634179,0.863989726799347,
244.886209595194));
#15220=CARTESIAN_POINT('Ctrl Pts',(-0.833555643942435,0.792051099534275,
244.886209595194));
#15221=CARTESIAN_POINT('Ctrl Pts',(-0.919110777044865,0.721817091729095,
244.886209595194));
#15222=CARTESIAN_POINT('Ctrl Pts',(-0.939073282913979,0.705429450892353,
244.886209595194));
#15223=CARTESIAN_POINT('Ctrl Pts',(-0.959119055207817,0.689134631185304,
244.886209595194));
#15224=CARTESIAN_POINT('Ctrl Pts',(-0.979247479859861,0.672933409900972,
244.886209595194));
#15225=CARTESIAN_POINT('Ctrl Pts',(-0.99876603580836,0.65722306746043,244.886209595194));
#15226=CARTESIAN_POINT('Ctrl Pts',(-1.01835549032636,0.641606244551321,
244.886209595194));
#15227=CARTESIAN_POINT('Ctrl Pts',(-1.03801184223114,0.626086015887525,
244.886209595194));
#15228=CARTESIAN_POINT('Ctrl Pts',(-1.20034525043236,0.497911081532396,
244.886209595194));
#15229=CARTESIAN_POINT('Ctrl Pts',(-1.3673109959342,0.376262636287241,244.886209595194));
#15230=CARTESIAN_POINT('Ctrl Pts',(-1.53852458201047,0.261404864848448,
244.886209595194));
#15231=CARTESIAN_POINT('Ctrl Pts',(-1.70927208788747,0.146859760962659,
244.886209595194));
#15232=CARTESIAN_POINT('Ctrl Pts',(-1.88424496013289,0.0390680863175076,
244.886209595194));
#15233=CARTESIAN_POINT('Ctrl Pts',(-2.06308629552965,-0.0616626459374319,
244.886209595194));
#15234=CARTESIAN_POINT('Ctrl Pts',(-2.23946463511152,-0.161006118522091,
244.886209595194));
#15235=CARTESIAN_POINT('Ctrl Pts',(-2.41960621621606,-0.253482007969893,
244.886209595194));
#15236=CARTESIAN_POINT('Ctrl Pts',(-2.60318342048835,-0.338747200573998,
244.886209595194));
#15237=CARTESIAN_POINT('Ctrl Pts',(-2.70012537870016,-0.383773350586004,
244.886209595194));
#15238=CARTESIAN_POINT('Ctrl Pts',(-2.7980255886567,-0.426787896006235,
244.886209595194));
#15239=CARTESIAN_POINT('Ctrl Pts',(-2.89683665674224,-0.467734470423956,
244.886209595194));
#15240=CARTESIAN_POINT('Ctrl Pts',(-3.04097870853666,-0.527465868584872,
244.886209595194));
#15241=CARTESIAN_POINT('Ctrl Pts',(-3.18705923438264,-0.582797331497136,
244.886209595194));
#15242=CARTESIAN_POINT('Ctrl Pts',(-3.33486953849687,-0.633661156473034,
244.886209595194));
#15243=CARTESIAN_POINT('Ctrl Pts',(-3.39953654654684,-0.655914079899989,
244.886209595194));
#15244=CARTESIAN_POINT('Ctrl Pts',(-3.46453462393422,-0.677311646689401,
244.886209595194));
#15245=CARTESIAN_POINT('Ctrl Pts',(-3.52984613578212,-0.697847143289031,
244.886209595194));
#15246=CARTESIAN_POINT('Ctrl Pts',(-3.56516437852512,-0.708952040928562,
244.886209595194));
#15247=CARTESIAN_POINT('Ctrl Pts',(-3.60057427600938,-0.719804834255837,
244.886209595194));
#15248=CARTESIAN_POINT('Ctrl Pts',(-3.63607302111687,-0.730404383715522,
244.886209595194));
#15249=CARTESIAN_POINT('Ctrl Pts',(-3.65875876597319,-0.73717810695296,
244.886209595194));
#15250=CARTESIAN_POINT('Ctrl Pts',(-3.68148075176679,-0.743848346809334,
244.886209595194));
#15251=CARTESIAN_POINT('Ctrl Pts',(-3.70422452712716,-0.750410975276562,
244.886209595194));
#15252=CARTESIAN_POINT('Ctrl Pts',(-3.8972186286978,-0.806098677292012,
244.886209595194));
#15253=CARTESIAN_POINT('Ctrl Pts',(-4.0920279033681,-0.854116647242459,
244.886209595194));
#15254=CARTESIAN_POINT('Ctrl Pts',(-4.28819139577941,-0.894431540392954,
244.886209595194));
#15255=CARTESIAN_POINT('Ctrl Pts',(-4.48469632720638,-0.934816604997193,
244.886209595194));
#15256=CARTESIAN_POINT('Ctrl Pts',(-4.68256091287849,-0.967471782307452,
244.886209595194));
#15257=CARTESIAN_POINT('Ctrl Pts',(-4.88132713130532,-0.992311928479702,
244.886209595194));
#15258=CARTESIAN_POINT('Ctrl Pts',(-5.07865800431528,-1.01697269713878,
244.886209595194));
#15259=CARTESIAN_POINT('Ctrl Pts',(-5.27687821507438,-1.03393085364646,
244.886209595194));
#15260=CARTESIAN_POINT('Ctrl Pts',(-5.47553442148217,-1.04305246810537,
244.886209595194));
#15261=CARTESIAN_POINT('Ctrl Pts',(-5.67013106277854,-1.0519876812004,244.886209595194));
#15262=CARTESIAN_POINT('Ctrl Pts',(-5.86514663500213,-1.05340321878937,
244.886209595194));
#15263=CARTESIAN_POINT('Ctrl Pts',(-6.06014087521336,-1.04712598159856,
244.886209595194));
#15264=CARTESIAN_POINT('Ctrl Pts',(-6.22877466971413,-1.04169733752517,
244.886209595194));
#15265=CARTESIAN_POINT('Ctrl Pts',(-6.39739251603998,-1.03051451432944,
244.886209595194));
#15266=CARTESIAN_POINT('Ctrl Pts',(-6.56569596473014,-1.01343717499105,
244.886209595194));
#15267=CARTESIAN_POINT('Ctrl Pts',(-15.3655110343894,6.43162198763813,245.944594374291));
#15268=CARTESIAN_POINT('Ctrl Pts',(-15.3649309294981,7.34903226064943,245.903429071413));
#15269=CARTESIAN_POINT('Ctrl Pts',(-15.2231421086117,8.26661783103502,245.862263768536));
#15270=CARTESIAN_POINT('Ctrl Pts',(-14.9430580168295,9.13984595302551,245.821098465658));
#15271=CARTESIAN_POINT('Ctrl Pts',(-14.5008015642581,10.5186846048734,245.756097912775));
#15272=CARTESIAN_POINT('Ctrl Pts',(-13.7137359469425,11.7869276113877,245.691097359891));
#15273=CARTESIAN_POINT('Ctrl Pts',(-12.6745084880691,12.7952885109223,245.626096807008));
#15274=CARTESIAN_POINT('Ctrl Pts',(-11.6352810291958,13.8036494104569,245.561096254125));
#15275=CARTESIAN_POINT('Ctrl Pts',(-10.3438917287647,14.5521282030119,245.496095701242));
#15276=CARTESIAN_POINT('Ctrl Pts',(-8.95234825169469,14.952622332577,245.431095148358));
#15277=CARTESIAN_POINT('Ctrl Pts',(-7.56080477462465,15.353116462142,245.366094595475));
#15278=CARTESIAN_POINT('Ctrl Pts',(-6.06910712091566,15.4056259287171,245.301094042592));
#15279=CARTESIAN_POINT('Ctrl Pts',(-4.65285002454947,15.1039668087614,245.236093489709));
#15280=CARTESIAN_POINT('Ctrl Pts',(-3.23659292818328,14.8023076888057,245.171092936825));
#15281=CARTESIAN_POINT('Ctrl Pts',(-1.89577638915989,14.1464799823193,245.106092383942));
#15282=CARTESIAN_POINT('Ctrl Pts',(-0.788216045743495,13.2136886030676,
245.041091831059));
#15283=CARTESIAN_POINT('Ctrl Pts',(0.0914760734497426,12.4728086771505,
244.989464419104));
#15284=CARTESIAN_POINT('Ctrl Pts',(0.82401835200515,11.5572060168434,244.937837007149));
#15285=CARTESIAN_POINT('Ctrl Pts',(1.35783022118007,10.5382254078893,244.886209595194));
#15286=CARTESIAN_POINT('',(-10.823035578903,12.4936896459292,258.886209595194));
#15287=CARTESIAN_POINT('Ctrl Pts',(-10.8232424565741,12.4936870253197,258.886209595194));
#15288=CARTESIAN_POINT('Ctrl Pts',(-10.9962627591582,12.3931877738435,258.886209595194));
#15289=CARTESIAN_POINT('Ctrl Pts',(-11.1648792140985,12.2858828094393,258.886209595194));
#15290=CARTESIAN_POINT('Ctrl Pts',(-11.3286727627758,12.1720546999129,258.886209595194));
#15291=CARTESIAN_POINT('Ctrl Pts',(-11.3719609836911,12.1419716081713,258.886209595194));
#15292=CARTESIAN_POINT('Ctrl Pts',(-11.414912325497,12.1114326134579,258.886209595194));
#15293=CARTESIAN_POINT('Ctrl Pts',(-11.4575189940443,12.0804423304784,258.886209595194));
#15294=CARTESIAN_POINT('Ctrl Pts',(-11.6170775755966,11.9643861880317,258.886209595194));
#15295=CARTESIAN_POINT('Ctrl Pts',(-11.7718036894195,11.8420049310846,258.886209595194));
#15296=CARTESIAN_POINT('Ctrl Pts',(-11.9214743026385,11.7137318538276,258.886209595194));
#15297=CARTESIAN_POINT('Ctrl Pts',(-12.0728964758752,11.5839576268885,258.886209595194));
#15298=CARTESIAN_POINT('Ctrl Pts',(-12.2191446525058,11.4481525108327,258.886209595194));
#15299=CARTESIAN_POINT('Ctrl Pts',(-12.3599656903401,11.3067164015234,258.886209595194));
#15300=CARTESIAN_POINT('Ctrl Pts',(-12.5014891650213,11.1645747872969,258.886209595194));
#15301=CARTESIAN_POINT('Ctrl Pts',(-12.637531758463,11.0167454229121,258.886209595194));
#15302=CARTESIAN_POINT('Ctrl Pts',(-12.7678062758748,10.8635913652864,258.886209595194));
#15303=CARTESIAN_POINT('Ctrl Pts',(-12.8215172612427,10.800447355916,258.886209595194));
#15304=CARTESIAN_POINT('Ctrl Pts',(-12.8742473673171,10.7363977711965,258.886209595194));
#15305=CARTESIAN_POINT('Ctrl Pts',(-12.925974648325,10.6714662234646,258.886209595194));
#15306=CARTESIAN_POINT('Ctrl Pts',(-12.9487466877829,10.6428812343022,258.886209595194));
#15307=CARTESIAN_POINT('Ctrl Pts',(-12.9713243599966,10.6141253035477,258.886209595194));
#15308=CARTESIAN_POINT('Ctrl Pts',(-12.9937057199584,10.5852003868364,258.886209595194));
#15309=CARTESIAN_POINT('Ctrl Pts',(-13.0094132693077,10.5649004784554,258.886209595194));
#15310=CARTESIAN_POINT('Ctrl Pts',(-13.0250248889854,10.5445162521638,258.886209595194));
#15311=CARTESIAN_POINT('Ctrl Pts',(-13.0405290850171,10.52406286367,258.886209595194));
#15312=CARTESIAN_POINT('Ctrl Pts',(-13.1640791364024,10.3610736190649,258.886209595194));
#15313=CARTESIAN_POINT('Ctrl Pts',(-13.28096895391,10.19349218881,258.886209595194));
#15314=CARTESIAN_POINT('Ctrl Pts',(-13.3909685719566,10.0217722607569,258.886209595194));
#15315=CARTESIAN_POINT('Ctrl Pts',(-13.5021881043256,9.84814792973064,258.886209595194));
#15316=CARTESIAN_POINT('Ctrl Pts',(-13.6063643146254,9.67029237005731,258.886209595194));
#15317=CARTESIAN_POINT('Ctrl Pts',(-13.7032312620926,9.48862953956923,258.886209595194));
#15318=CARTESIAN_POINT('Ctrl Pts',(-13.7537935981977,9.39380568754212,258.886209595194));
#15319=CARTESIAN_POINT('Ctrl Pts',(-13.802363935953,9.2979438059089,258.886209595194));
#15320=CARTESIAN_POINT('Ctrl Pts',(-13.8489006720425,9.20110001266742,258.886209595194));
#15321=CARTESIAN_POINT('Ctrl Pts',(-13.9375249912023,9.0166711944459,258.886209595194));
#15322=CARTESIAN_POINT('Ctrl Pts',(-14.0187767861329,8.828682979896,258.886209595194));
#15323=CARTESIAN_POINT('Ctrl Pts',(-14.0926202070319,8.63760482503333,258.886209595194));
#15324=CARTESIAN_POINT('Ctrl Pts',(-14.1425987595604,8.50827970055252,258.886209595194));
#15325=CARTESIAN_POINT('Ctrl Pts',(-14.1891827861434,8.37753843385314,258.886209595194));
#15326=CARTESIAN_POINT('Ctrl Pts',(-14.2323493892896,8.24551998345277,258.886209595194));
#15327=CARTESIAN_POINT('Ctrl Pts',(-14.2701201670426,8.13000383935244,258.886209595194));
#15328=CARTESIAN_POINT('Ctrl Pts',(-14.3052743501943,8.01350973685049,258.886209595194));
#15329=CARTESIAN_POINT('Ctrl Pts',(-14.3377902985068,7.89612836485591,258.886209595194));
#15330=CARTESIAN_POINT('Ctrl Pts',(-14.346429637234,7.86494067126071,258.886209595194));
#15331=CARTESIAN_POINT('Ctrl Pts',(-14.3548838005409,7.83368591534596,258.886209595194));
#15332=CARTESIAN_POINT('Ctrl Pts',(-14.3631450505409,7.80239401210579,258.886209595194));
#15333=CARTESIAN_POINT('Ctrl Pts',(-14.4166320128683,7.59979648149569,258.886209595194));
#15334=CARTESIAN_POINT('Ctrl Pts',(-14.4620953012549,7.39543822996992,258.886209595194));
#15335=CARTESIAN_POINT('Ctrl Pts',(-14.4995572873584,7.18983840967408,258.886209595194));
#15336=CARTESIAN_POINT('Ctrl Pts',(-14.5373634910809,6.98234944552973,258.886209595194));
#15337=CARTESIAN_POINT('Ctrl Pts',(-14.56702093691,6.77359537785523,258.886209595194));
#15338=CARTESIAN_POINT('Ctrl Pts',(-14.5885083677775,6.56407930036393,258.886209595194));
#15339=CARTESIAN_POINT('Ctrl Pts',(-14.6100583701105,6.35395311140345,258.886209595194));
#15340=CARTESIAN_POINT('Ctrl Pts',(-14.6233909328497,6.14305979808593,258.886209595194));
#15341=CARTESIAN_POINT('Ctrl Pts',(-14.6284367109836,5.93188605522641,258.886209595194));
#15342=CARTESIAN_POINT('Ctrl Pts',(-14.6328908783898,5.74547215086212,258.886209595194));
#15343=CARTESIAN_POINT('Ctrl Pts',(-14.6308869777452,5.55883911524171,258.886209595194));
#15344=CARTESIAN_POINT('Ctrl Pts',(-14.6223442849833,5.37231468247016,258.886209595194));
#15345=CARTESIAN_POINT('Ctrl Pts',(-14.6145158995427,5.2013867099297,258.886209595194));
#15346=CARTESIAN_POINT('Ctrl Pts',(-14.6011961461742,5.03054965713793,258.886209595194));
#15347=CARTESIAN_POINT('Ctrl Pts',(-14.5824613743046,4.86003478198579,258.886209595194));
#15348=CARTESIAN_POINT('Ctrl Pts',(-14.5785562001578,4.82449176674548,258.886209595194));
#15349=CARTESIAN_POINT('Ctrl Pts',(-14.5744156684306,4.78896275492112,258.886209595194));
#15350=CARTESIAN_POINT('Ctrl Pts',(-14.5700403476506,4.75344985240902,258.886209595194));
#15351=CARTESIAN_POINT('Ctrl Pts',(-14.5670822017472,4.72943964781649,258.886209595194));
#15352=CARTESIAN_POINT('Ctrl Pts',(-14.5640167675075,4.70543742739751,258.886209595194));
#15353=CARTESIAN_POINT('Ctrl Pts',(-14.5608460966616,4.68145708463058,258.886209595194));
#15354=CARTESIAN_POINT('Ctrl Pts',(-14.5330800108368,4.47145728088453,258.886209595194));
#15355=CARTESIAN_POINT('Ctrl Pts',(-14.4972158831587,4.26287242485888,258.886209595194));
#15356=CARTESIAN_POINT('Ctrl Pts',(-14.4535260619027,4.0561402580423,258.886209595194));
#15357=CARTESIAN_POINT('Ctrl Pts',(-14.4091822964983,3.84631374826656,258.886209595194));
#15358=CARTESIAN_POINT('Ctrl Pts',(-14.3567768109032,3.63839520345404,258.886209595194));
#15359=CARTESIAN_POINT('Ctrl Pts',(-14.2965417977189,3.43283197016907,258.886209595194));
#15360=CARTESIAN_POINT('Ctrl Pts',(-14.2356273487361,3.22495003531564,258.886209595194));
#15361=CARTESIAN_POINT('Ctrl Pts',(-14.1667057060184,3.01947617599251,258.886209595194));
#15362=CARTESIAN_POINT('Ctrl Pts',(-14.0899640341328,2.81687222565179,258.886209595194));
#15363=CARTESIAN_POINT('Ctrl Pts',(-14.0133154717191,2.61451409151968,258.886209595194));
#15364=CARTESIAN_POINT('Ctrl Pts',(-13.9288656987432,2.4150182161233,258.886209595194));
#15365=CARTESIAN_POINT('Ctrl Pts',(-13.8367502112676,2.21885418100079,258.886209595194));
#15366=CARTESIAN_POINT('Ctrl Pts',(-13.7773429727528,2.09234381947636,258.886209595194));
#15367=CARTESIAN_POINT('Ctrl Pts',(-13.7147463578949,1.96721946515344,258.886209595194));
#15368=CARTESIAN_POINT('Ctrl Pts',(-13.6489858644575,1.8436112222596,258.886209595194));
#15369=CARTESIAN_POINT('Ctrl Pts',(-13.6273871639318,1.80301272183439,258.886209595194));
#15370=CARTESIAN_POINT('Ctrl Pts',(-13.6054470896328,1.76257780630002,258.886209595194));
#15371=CARTESIAN_POINT('Ctrl Pts',(-13.5831663497552,1.7223111889938,258.886209595194));
#15372=CARTESIAN_POINT('Ctrl Pts',(-13.5703103265728,1.69907728525407,258.886209595194));
#15373=CARTESIAN_POINT('Ctrl Pts',(-13.5573395664917,1.67589709266456,258.886209595194));
#15374=CARTESIAN_POINT('Ctrl Pts',(-13.5442586020083,1.652779302687,258.886209595194));
#15375=CARTESIAN_POINT('Ctrl Pts',(-13.5109861443909,1.59397739337683,258.886209595194));
#15376=CARTESIAN_POINT('Ctrl Pts',(-13.4770141268117,1.53560253787742,258.886209595194));
#15377=CARTESIAN_POINT('Ctrl Pts',(-13.4423489066022,1.47766813376721,258.886209595194));
#15378=CARTESIAN_POINT('Ctrl Pts',(-13.3304954334553,1.29073251716748,258.886209595194));
#15379=CARTESIAN_POINT('Ctrl Pts',(-13.2114286638561,1.10838157575998,258.886209595194));
#15380=CARTESIAN_POINT('Ctrl Pts',(-13.0855785738617,0.930887529340759,
258.886209595194));
#15381=CARTESIAN_POINT('Ctrl Pts',(-12.9582535083845,0.75131323516952,258.886209595194));
#15382=CARTESIAN_POINT('Ctrl Pts',(-12.8239848789003,0.576709821915435,
258.886209595194));
#15383=CARTESIAN_POINT('Ctrl Pts',(-12.683167458968,0.407377372868322,258.886209595194));
#15384=CARTESIAN_POINT('Ctrl Pts',(-12.6043188879753,0.312562245333209,
258.886209595194));
#15385=CARTESIAN_POINT('Ctrl Pts',(-12.5234162183088,0.219400076748213,
258.886209595194));
#15386=CARTESIAN_POINT('Ctrl Pts',(-12.4405225347237,0.127946949428894,
258.886209595194));
#15387=CARTESIAN_POINT('Ctrl Pts',(-12.3755960071966,0.0563162324484651,
258.886209595194));
#15388=CARTESIAN_POINT('Ctrl Pts',(-12.3094479391927,-0.0142659736946958,
258.886209595194));
#15389=CARTESIAN_POINT('Ctrl Pts',(-12.2421069024936,-0.0837714615598565,
258.886209595194));
#15390=CARTESIAN_POINT('Ctrl Pts',(-12.2202634288917,-0.106317020164007,
258.886209595194));
#15391=CARTESIAN_POINT('Ctrl Pts',(-12.1982941806089,-0.128749454165727,
258.886209595194));
#15392=CARTESIAN_POINT('Ctrl Pts',(-12.1762108309938,-0.15105715093638,
258.886209595194));
#15393=CARTESIAN_POINT('Ctrl Pts',(-12.0183040784386,-0.310568095400722,
258.886209595194));
#15394=CARTESIAN_POINT('Ctrl Pts',(-11.8544368053254,-0.463838871245082,
258.886209595194));
#15395=CARTESIAN_POINT('Ctrl Pts',(-11.6850343963611,-0.610571371251755,
258.886209595194));
#15396=CARTESIAN_POINT('Ctrl Pts',(-11.5148563117381,-0.757975743809088,
258.886209595194));
#15397=CARTESIAN_POINT('Ctrl Pts',(-11.3390918710149,-0.898782372462146,
258.886209595194));
#15398=CARTESIAN_POINT('Ctrl Pts',(-11.1581273042666,-1.03266178326809,
258.886209595194));
#15399=CARTESIAN_POINT('Ctrl Pts',(-10.97782946116,-1.16604794520257,258.886209595194));
#15400=CARTESIAN_POINT('Ctrl Pts',(-10.7923692685769,-1.29255835071171,
258.886209595194));
#15401=CARTESIAN_POINT('Ctrl Pts',(-10.6020908326724,-1.41183230447377,
258.886209595194));
#15402=CARTESIAN_POINT('Ctrl Pts',(-10.5494809025752,-1.44481026301129,
258.886209595194));
#15403=CARTESIAN_POINT('Ctrl Pts',(-10.4965024352886,-1.47723479084939,
258.886209595194));
#15404=CARTESIAN_POINT('Ctrl Pts',(-10.4431622648007,-1.50909770983434,
258.886209595194));
#15405=CARTESIAN_POINT('Ctrl Pts',(-10.8232424565743,12.4936870253196,258.886209595194));
#15406=CARTESIAN_POINT('Ctrl Pts',(-10.0361782840362,13.0538187692527,258.834582183239));
#15407=CARTESIAN_POINT('Ctrl Pts',(-8.01076733182417,13.973648670065,258.7179542184));
#15408=CARTESIAN_POINT('Ctrl Pts',(-4.50862938937823,13.9217796100182,258.536325700679));
#15409=CARTESIAN_POINT('Ctrl Pts',(-1.21743004662297,12.1027648942659,258.341324042029));
#15410=CARTESIAN_POINT('Ctrl Pts',(0.830132802421682,8.94868564322478,258.146322383379));
#15411=CARTESIAN_POINT('Ctrl Pts',(1.15202784967473,5.20206719240598,257.951320724729));
#15412=CARTESIAN_POINT('Ctrl Pts',(-0.327530058757188,1.74494971672666,
257.75631906608));
#15413=CARTESIAN_POINT('Ctrl Pts',(-3.26021932302907,-0.608789762765702,
257.56131740743));
#15414=CARTESIAN_POINT('Ctrl Pts',(-6.95562279721707,-1.30502921472525,
257.36631574878));
#15415=CARTESIAN_POINT('Ctrl Pts',(-10.5437627550554,-0.179859485232368,
257.17131409013));
#15416=CARTESIAN_POINT('Ctrl Pts',(-13.1799141928899,2.50183057058523,256.976312431481));
#15417=CARTESIAN_POINT('Ctrl Pts',(-13.9191133736988,5.00870786476085,256.840781211995));
#15418=CARTESIAN_POINT('Ctrl Pts',(-13.946066322283,6.32821536422246,256.770250545393));
#15419=CARTESIAN_POINT('Ctrl Pts',(-13.9459987791106,6.43167704459545,256.764720431675));
#15420=CARTESIAN_POINT('Origin',(-6.5,6.43177298256785,263.507698758713));
#15421=CARTESIAN_POINT('',(-2.17696442109693,12.4936896459292,258.886209595194));
#15422=CARTESIAN_POINT('Origin',(-6.5,6.43177298256785,258.886209595194));
#15423=CARTESIAN_POINT('Ctrl Pts',(-2.17696442109716,12.4936896459294,258.886209595194));
#15424=CARTESIAN_POINT('Ctrl Pts',(-1.18666420925076,11.7874603644412,258.82120904231));
#15425=CARTESIAN_POINT('Ctrl Pts',(0.440228799577828,9.88095277329113,258.691207936544));
#15426=CARTESIAN_POINT('Ctrl Pts',(1.24700262019175,6.20780816435965,258.496206277894));
#15427=CARTESIAN_POINT('Ctrl Pts',(0.229685845340515,2.58777411101262,258.301204619244));
#15428=CARTESIAN_POINT('Ctrl Pts',(-2.37185181727327,-0.127533036464177,
258.106202960595));
#15429=CARTESIAN_POINT('Ctrl Pts',(-5.94529650349566,-1.29854737465037,
257.911201301945));
#15430=CARTESIAN_POINT('Ctrl Pts',(-9.64930901441413,-0.649724643295287,
257.716199643295));
#15431=CARTESIAN_POINT('Ctrl Pts',(-12.6119171141539,1.66625481118851,257.521197984645));
#15432=CARTESIAN_POINT('Ctrl Pts',(-13.8061465224486,4.36070848620917,257.368364356451));
#15433=CARTESIAN_POINT('Ctrl Pts',(-13.9454232283679,6.00432209899089,257.280531281141));
#15434=CARTESIAN_POINT('Ctrl Pts',(-13.9451274702829,6.4316349637354,257.257698758713));
#15435=CARTESIAN_POINT('Ctrl Pts',(-1.35218810791047,13.6502207882711,259.706335652578));
#15436=CARTESIAN_POINT('Ctrl Pts',(-0.17295210250719,12.8092525779865,259.641335099694));
#15437=CARTESIAN_POINT('Ctrl Pts',(1.7643299358078,10.5390093031041,259.511333993928));
#15438=CARTESIAN_POINT('Ctrl Pts',(2.72502521397086,6.16507872721444,259.316332335278));
#15439=CARTESIAN_POINT('Ctrl Pts',(1.51361825327903,1.85439147760396,259.121330676628));
#15440=CARTESIAN_POINT('Ctrl Pts',(-1.58425736511246,-1.37895929393983,
258.926329017979));
#15441=CARTESIAN_POINT('Ctrl Pts',(-5.83946663084983,-2.77338721984928,
258.731327359329));
#15442=CARTESIAN_POINT('Ctrl Pts',(-10.2501542840368,-2.00077794764538,
258.536325700679));
#15443=CARTESIAN_POINT('Ctrl Pts',(-13.7779876615523,0.757058845512007,
258.341324042029));
#15444=CARTESIAN_POINT('Ctrl Pts',(-15.5924209408393,4.85083377978987,258.146322383379));
#15445=CARTESIAN_POINT('Ctrl Pts',(-15.2663057152418,9.3168008922508,257.951320724729));
#15446=CARTESIAN_POINT('Ctrl Pts',(-12.8764127146944,13.1035680934288,257.75631906608));
#15447=CARTESIAN_POINT('Ctrl Pts',(-8.98537579921665,15.3196525658886,257.56131740743));
#15448=CARTESIAN_POINT('Ctrl Pts',(-4.50922780436335,15.443338842549,257.36631574878));
#15449=CARTESIAN_POINT('Ctrl Pts',(-0.501750445330013,13.4455092555275,
257.17131409013));
#15450=CARTESIAN_POINT('Ctrl Pts',(2.09361023016663,9.7964954472964,256.976312431481));
#15451=CARTESIAN_POINT('Ctrl Pts',(2.66585051492385,5.35535377421556,256.781310772831));
#15452=CARTESIAN_POINT('Ctrl Pts',(1.08025279484469,1.16762427255162,256.586309114181));
#15453=CARTESIAN_POINT('Ctrl Pts',(-2.28989919801298,-1.78081158301322,
256.391307455531));
#15454=CARTESIAN_POINT('Ctrl Pts',(-6.65119931460797,-2.79582869980662,
256.196305796881));
#15455=CARTESIAN_POINT('Ctrl Pts',(-10.9769038671609,-1.63847024757435,
256.001304138232));
#15456=CARTESIAN_POINT('Ctrl Pts',(-14.24864912287,1.41879674055062,255.806302479582));
#15457=CARTESIAN_POINT('Ctrl Pts',(-15.6961959998786,5.65622597281891,255.611300820932));
#15458=CARTESIAN_POINT('Ctrl Pts',(-14.9787608819424,10.0762356231545,255.416299162282));
#15459=CARTESIAN_POINT('Ctrl Pts',(-12.2652434004147,13.6382605157787,255.221297503632));
#15460=CARTESIAN_POINT('Ctrl Pts',(-8.19446383376755,15.5037235086731,255.026295844983));
#15461=CARTESIAN_POINT('Ctrl Pts',(-3.7247710979183,15.2334545590181,254.831294186333));
#15462=CARTESIAN_POINT('Ctrl Pts',(0.0915731659545367,12.891080780622,254.636292527683));
#15463=CARTESIAN_POINT('Ctrl Pts',(2.3561195753497,9.02804725529935,254.441290869033));
#15464=CARTESIAN_POINT('Ctrl Pts',(2.53574528220585,4.55379502017353,254.246289210384));
#15465=CARTESIAN_POINT('Ctrl Pts',(0.588162538287489,0.521659120470325,
254.051287551734));
#15466=CARTESIAN_POINT('Ctrl Pts',(-3.02812586089059,-2.11910907686471,
253.856285893084));
#15467=CARTESIAN_POINT('Ctrl Pts',(-7.46176797889057,-2.74681603682514,
253.661284234434));
#15468=CARTESIAN_POINT('Ctrl Pts',(-11.6689892640225,-1.21368606320314,
253.466282575784));
#15469=CARTESIAN_POINT('Ctrl Pts',(-14.6593194902573,2.11934912955326,253.271280917135));
#15470=CARTESIAN_POINT('Ctrl Pts',(-15.7287707153518,6.46762149167933,253.076279258485));
#15471=CARTESIAN_POINT('Ctrl Pts',(-14.625571158157,10.807454345038,252.881277599835));
#15472=CARTESIAN_POINT('Ctrl Pts',(-11.609437681827,14.1171578530651,252.686275941185));
#15473=CARTESIAN_POINT('Ctrl Pts',(-7.39043286771254,15.6175567455485,252.491274282535));
#15474=CARTESIAN_POINT('Ctrl Pts',(-2.96180103757599,14.9554249073266,252.296272623886));
#15475=CARTESIAN_POINT('Ctrl Pts',(0.63386278623459,12.2866423901053,252.101270965236));
#15476=CARTESIAN_POINT('Ctrl Pts',(2.55006213516392,8.23949790130234,251.906269306586));
#15477=CARTESIAN_POINT('Ctrl Pts',(2.33568253872803,3.76677615199603,251.711267647936));
#15478=CARTESIAN_POINT('Ctrl Pts',(0.0411935569874599,-0.0785481218145621,
251.516265989287));
#15479=CARTESIAN_POINT('Ctrl Pts',(-3.79323283755008,-2.39120302105044,
251.321264330637));
#15480=CARTESIAN_POINT('Ctrl Pts',(-8.26489034058072,-2.6267399261753,251.126262671987));
#15481=CARTESIAN_POINT('Ctrl Pts',(-12.3210547625296,-0.729708392383273,
250.931261013337));
#15482=CARTESIAN_POINT('Ctrl Pts',(-15.0068179063841,2.85328962508741,250.736259354687));
#15483=CARTESIAN_POINT('Ctrl Pts',(-15.6898934606167,7.27873946044833,250.541257696038));
#15484=CARTESIAN_POINT('Ctrl Pts',(-14.2094707730794,11.5047952012436,250.346256037388));
#15485=CARTESIAN_POINT('Ctrl Pts',(-10.9140731313682,14.5365525861766,250.151254378738));
#15486=CARTESIAN_POINT('Ctrl Pts',(-6.57950789759873,15.660270830341,249.956252720088));
#15487=CARTESIAN_POINT('Ctrl Pts',(-2.22622479757299,14.6114025311045,249.761251061438));
#15488=CARTESIAN_POINT('Ctrl Pts',(1.12091985526713,11.6368738069172,249.566249402789));
#15489=CARTESIAN_POINT('Ctrl Pts',(2.67393634133375,7.43695258716843,249.371247744139));
#15490=CARTESIAN_POINT('Ctrl Pts',(2.06721123408506,3.00039050572924,249.176246085489));
#15491=CARTESIAN_POINT('Ctrl Pts',(-0.556419348759181,-0.628350463570228,
248.981244426839));
#15492=CARTESIAN_POINT('Ctrl Pts',(-4.57929643494695,-2.59498678201968,
248.786242768189));
#15493=CARTESIAN_POINT('Ctrl Pts',(-9.05434838031283,-2.43653003331118,
248.59124110954));
#15494=CARTESIAN_POINT('Ctrl Pts',(-12.9280518722398,-0.190284338921679,
248.39623945089));
#15495=CARTESIAN_POINT('Ctrl Pts',(-15.2884539309517,3.6149358354734,248.20123779224));
#15496=CARTESIAN_POINT('Ctrl Pts',(-15.5798652377731,8.08329995443233,248.00623613359));
#15497=CARTESIAN_POINT('Ctrl Pts',(-13.7336812979301,12.1628591670547,247.811234474941));
#15498=CARTESIAN_POINT('Ctrl Pts',(-10.184533486267,14.8931976286455,247.616232816291));
#15499=CARTESIAN_POINT('Ctrl Pts',(-5.767967327236,15.6315350660532,247.421231157641));
#15500=CARTESIAN_POINT('Ctrl Pts',(-1.5237374905245,14.2040509382567,247.226229498991));
#15501=CARTESIAN_POINT('Ctrl Pts',(1.54897354961792,10.9468057785166,247.031227840341));
#15502=CARTESIAN_POINT('Ctrl Pts',(2.72678285689953,6.6266247750899,246.836226181692));
#15503=CARTESIAN_POINT('Ctrl Pts',(1.73241052921659,2.26057185924915,246.641224523042));
#15504=CARTESIAN_POINT('Ctrl Pts',(-1.20005053150349,-1.12349160311523,
246.446222864392));
#15505=CARTESIAN_POINT('Ctrl Pts',(-5.38022800707743,-2.72888177693902,
246.251221205742));
#15506=CARTESIAN_POINT('Ctrl Pts',(-9.82403584101992,-2.17766126553081,
246.056219547092));
#15507=CARTESIAN_POINT('Ctrl Pts',(-13.485268418384,0.4004129529351,245.861217888443));
#15508=CARTESIAN_POINT('Ctrl Pts',(-15.5020757887051,4.39837783106898,245.666216229793));
#15509=CARTESIAN_POINT('Ctrl Pts',(-15.3994802353216,8.87508026827576,245.471214571143));
#15510=CARTESIAN_POINT('Ctrl Pts',(-13.2020294654162,12.7764571408952,245.276212912493));
#15511=CARTESIAN_POINT('Ctrl Pts',(-9.42621760171243,15.1842463488826,245.081211253844));
#15512=CARTESIAN_POINT('Ctrl Pts',(-6.45069372495972,15.415165992917,244.951210148077));
#15513=CARTESIAN_POINT('Ctrl Pts',(-5.02255860044595,15.1738049495012,244.886209595194));
#15514=CARTESIAN_POINT('Ctrl Pts',(-1.62711354563937,13.2647104074905,259.432960300116));
#15515=CARTESIAN_POINT('Ctrl Pts',(-0.510856138088382,12.4686551734714,
259.367959747233));
#15516=CARTESIAN_POINT('Ctrl Pts',(1.32296289039781,10.3196571264998,259.237958641467));
#15517=CARTESIAN_POINT('Ctrl Pts',(2.23235101604449,6.17932187292951,259.042956982817));
#15518=CARTESIAN_POINT('Ctrl Pts',(1.08564078396619,2.09885235540685,258.847955324167));
#15519=CARTESIAN_POINT('Ctrl Pts',(-1.84678884916606,-0.96181720811461,
258.652953665517));
#15520=CARTESIAN_POINT('Ctrl Pts',(-5.87474325506511,-2.28177393811631,
258.457952006867));
#15521=CARTESIAN_POINT('Ctrl Pts',(-10.0498725274959,-1.55042684619535,
258.262950348218));
#15522=CARTESIAN_POINT('Ctrl Pts',(-13.3892974790862,1.06012416740417,258.067948689568));
#15523=CARTESIAN_POINT('Ctrl Pts',(-15.1068286426792,4.93526584752227,257.872947030918));
#15524=CARTESIAN_POINT('Ctrl Pts',(-14.7981300152456,9.16272230943613,257.677945372268));
#15525=CARTESIAN_POINT('Ctrl Pts',(-12.5358722883005,12.7472523946929,257.482943713619));
#15526=CARTESIAN_POINT('Ctrl Pts',(-8.8526411453785,14.8449840589292,257.287942054969));
#15527=CARTESIAN_POINT('Ctrl Pts',(-4.61554752403783,14.9620647127609,257.092940396319));
#15528=CARTESIAN_POINT('Ctrl Pts',(-0.82209458746133,13.0709317543718,256.897938737669));
#15529=CARTESIAN_POINT('Ctrl Pts',(1.63465755207235,9.61679816700663,256.702937079019));
#15530=CARTESIAN_POINT('Ctrl Pts',(2.1763366170199,5.41284131032596,256.50793542037));
#15531=CARTESIAN_POINT('Ctrl Pts',(0.675419758711259,1.44876282592323,256.31293376172));
#15532=CARTESIAN_POINT('Ctrl Pts',(-2.51474498300518,-1.34220806487623,
256.11793210307));
#15533=CARTESIAN_POINT('Ctrl Pts',(-6.64312432301459,-2.30301690231008,
255.92293044442));
#15534=CARTESIAN_POINT('Ctrl Pts',(-10.7378091253268,-1.2074686493934,255.72792878577));
#15535=CARTESIAN_POINT('Ctrl Pts',(-13.8348226667817,1.68652110899131,255.532927127121));
#15536=CARTESIAN_POINT('Ctrl Pts',(-15.205061462777,5.69764504670974,255.337925468471));
#15537=CARTESIAN_POINT('Ctrl Pts',(-14.5259418792806,9.88159846318187,255.142923809821));
#15538=CARTESIAN_POINT('Ctrl Pts',(-11.9573432481368,13.2533888885539,254.947922151171));
#15539=CARTESIAN_POINT('Ctrl Pts',(-8.10396883881053,15.0192244590328,254.752920492521));
#15540=CARTESIAN_POINT('Ctrl Pts',(-3.87298572516121,14.763389566186,254.557918833872));
#15541=CARTESIAN_POINT('Ctrl Pts',(-0.260458177839673,12.5461132369294,
254.362917175222));
#15542=CARTESIAN_POINT('Ctrl Pts',(1.88314725198763,8.88938992751473,254.167915516572));
#15543=CARTESIAN_POINT('Ctrl Pts',(2.05317981963823,4.65409082044352,253.972913857922));
#15544=CARTESIAN_POINT('Ctrl Pts',(0.209610207825143,0.837296263906278,
253.777912199273));
#15545=CARTESIAN_POINT('Ctrl Pts',(-3.21354571255632,-1.66243835104231,
253.582910540623));
#15546=CARTESIAN_POINT('Ctrl Pts',(-7.41040353742827,-2.25662182289749,
253.387908881973));
#15547=CARTESIAN_POINT('Ctrl Pts',(-11.392932821826,-0.805370604352179,
253.192907223323));
#15548=CARTESIAN_POINT('Ctrl Pts',(-14.2235606611757,2.34965960715335,252.997905564673));
#15549=CARTESIAN_POINT('Ctrl Pts',(-15.2358964841631,6.46570695648147,252.802903906024));
#15550=CARTESIAN_POINT('Ctrl Pts',(-14.1916147016504,10.5737655197357,252.607902247374));
#15551=CARTESIAN_POINT('Ctrl Pts',(-11.3365616675764,13.706710104793,252.412900588724));
#15552=CARTESIAN_POINT('Ctrl Pts',(-7.34287816854021,15.1269782871939,252.217898930074));
#15553=CARTESIAN_POINT('Ctrl Pts',(-3.15076305073951,14.50020844146,252.022897271425));
#15554=CARTESIAN_POINT('Ctrl Pts',(0.252869775938848,11.9739556469891,251.827895612775));
#15555=CARTESIAN_POINT('Ctrl Pts',(2.06673206286523,8.14295405413105,251.632893954125));
#15556=CARTESIAN_POINT('Ctrl Pts',(1.86380168128525,3.90910369533865,251.437892295475));
#15557=CARTESIAN_POINT('Ctrl Pts',(-0.308147199749915,0.269143852347981,
251.242890636825));
#15558=CARTESIAN_POINT('Ctrl Pts',(-3.93779117856294,-1.92000077226708,
251.047888978175));
#15559=CARTESIAN_POINT('Ctrl Pts',(-8.17063412850482,-2.14295852957143,
250.852887319526));
#15560=CARTESIAN_POINT('Ctrl Pts',(-12.0101739335134,-0.347240376249803,
250.657885660876));
#15561=CARTESIAN_POINT('Ctrl Pts',(-14.5525004826674,3.04440307757636,250.462884002226));
#15562=CARTESIAN_POINT('Ctrl Pts',(-15.1990955186359,7.2335061390772,250.267882343576));
#15563=CARTESIAN_POINT('Ctrl Pts',(-13.7977366865632,11.2338640010921,250.072880684927));
#15564=CARTESIAN_POINT('Ctrl Pts',(-10.6783339448464,14.1037065290698,249.877879026277));
#15565=CARTESIAN_POINT('Ctrl Pts',(-6.57526167726115,15.1674111719922,249.682877367627));
#15566=CARTESIAN_POINT('Ctrl Pts',(-2.45447119486029,14.1745590175435,249.487875708977));
#15567=CARTESIAN_POINT('Ctrl Pts',(0.713914943077987,11.3588887809383,249.292874050327));
#15568=CARTESIAN_POINT('Ctrl Pts',(2.1839906095921,7.38326969265249,249.097872391678));
#15569=CARTESIAN_POINT('Ctrl Pts',(1.60966842793355,3.18364784870049,248.902870733028));
#15570=CARTESIAN_POINT('Ctrl Pts',(-0.873843828610586,-0.251295596465967,
248.707869074378));
#15571=CARTESIAN_POINT('Ctrl Pts',(-4.6818740503375,-2.1129012024424,248.512867415728));
#15572=CARTESIAN_POINT('Ctrl Pts',(-8.91793015810686,-1.96290703782069,
248.317865757078));
#15573=CARTESIAN_POINT('Ctrl Pts',(-12.5847535909962,0.16337504994876,248.122864098429));
#15574=CARTESIAN_POINT('Ctrl Pts',(-14.8190953773418,3.76537260393147,247.927862439779));
#15575=CARTESIAN_POINT('Ctrl Pts',(-15.0949434928954,7.99509805716436,247.732860781129));
#15576=CARTESIAN_POINT('Ctrl Pts',(-13.3473573531331,11.8567832243123,247.537859122479));
#15577=CARTESIAN_POINT('Ctrl Pts',(-9.98775629184481,14.441304489697,247.342857463829));
#15578=CARTESIAN_POINT('Ctrl Pts',(-5.80706246264698,15.1402100777236,247.14785580518));
#15579=CARTESIAN_POINT('Ctrl Pts',(-1.7895011154102,13.7889625543159,246.95285414653));
#15580=CARTESIAN_POINT('Ctrl Pts',(1.11910788576228,10.7056747127731,246.75785248788));
#15581=CARTESIAN_POINT('Ctrl Pts',(2.23401478981833,6.61621846742475,246.56285082923));
#15582=CARTESIAN_POINT('Ctrl Pts',(1.29274818028989,2.48334015745481,246.367849170581));
#15583=CARTESIAN_POINT('Ctrl Pts',(-1.4831010698898,-0.719993094055798,
246.172847511931));
#15584=CARTESIAN_POINT('Ctrl Pts',(-5.44003085375563,-2.23964536495769,
245.977845853281));
#15585=CARTESIAN_POINT('Ctrl Pts',(-9.64651148158805,-1.71786348564419,
245.782844194631));
#15586=CARTESIAN_POINT('Ctrl Pts',(-13.1122112791888,0.722525402070124,
245.587842535981));
#15587=CARTESIAN_POINT('Ctrl Pts',(-15.0213084882368,4.50697388388138,245.392840877332));
#15588=CARTESIAN_POINT('Ctrl Pts',(-14.9241921807959,8.74459233687685,245.197839218682));
#15589=CARTESIAN_POINT('Ctrl Pts',(-12.8440990625429,12.4376112183858,245.002837560032));
#15590=CARTESIAN_POINT('Ctrl Pts',(-9.26993923103672,14.7168093830638,244.807835901382));
#15591=CARTESIAN_POINT('Ctrl Pts',(-6.45332698925382,14.9353964699754,244.677834795616));
#15592=CARTESIAN_POINT('Ctrl Pts',(-5.10146323643611,14.7069256198888,244.612834242732));
#15593=CARTESIAN_POINT('Ctrl Pts',(-1.90203898336826,12.8792000267099,259.159584947655));
#15594=CARTESIAN_POINT('Ctrl Pts',(-0.84876017366957,12.1280577689563,259.094584394772));
#15595=CARTESIAN_POINT('Ctrl Pts',(0.881595844987819,10.1003049498954,258.964583289005));
#15596=CARTESIAN_POINT('Ctrl Pts',(1.73967681811812,6.19356501864459,258.769581630356));
#15597=CARTESIAN_POINT('Ctrl Pts',(0.657663314653353,2.34331323320973,258.574579971706));
#15598=CARTESIAN_POINT('Ctrl Pts',(-2.10932033321967,-0.544675122289394,
258.379578313056));
#15599=CARTESIAN_POINT('Ctrl Pts',(-5.91001987928038,-1.79016065638334,
258.184576654406));
#15600=CARTESIAN_POINT('Ctrl Pts',(-9.849590770955,-1.10007574474532,257.989574995756));
#15601=CARTESIAN_POINT('Ctrl Pts',(-13.00060729662,1.36318948929634,257.794573337106));
#15602=CARTESIAN_POINT('Ctrl Pts',(-14.6212363445191,5.01969791525466,257.599571678457));
#15603=CARTESIAN_POINT('Ctrl Pts',(-14.3299543152493,9.00864372662145,257.404570019807));
#15604=CARTESIAN_POINT('Ctrl Pts',(-12.1953318619067,12.390936695957,257.209568361157));
#15605=CARTESIAN_POINT('Ctrl Pts',(-8.71990649154034,14.3703155519697,257.014566702507));
#15606=CARTESIAN_POINT('Ctrl Pts',(-4.72186724371231,14.4807905829729,256.819565043858));
#15607=CARTESIAN_POINT('Ctrl Pts',(-1.14243872959264,12.6963542532161,256.624563385208));
#15608=CARTESIAN_POINT('Ctrl Pts',(1.17570487397806,9.43710088671688,256.429561726558));
#15609=CARTESIAN_POINT('Ctrl Pts',(1.68682271911594,5.47032884643636,256.234560067908));
#15610=CARTESIAN_POINT('Ctrl Pts',(0.270586722577831,1.72990137929484,256.039558409258));
#15611=CARTESIAN_POINT('Ctrl Pts',(-2.73959076799738,-0.903604546739227,
255.844556750609));
#15612=CARTESIAN_POINT('Ctrl Pts',(-6.63504933142122,-1.81020510481355,
255.649555091959));
#15613=CARTESIAN_POINT('Ctrl Pts',(-10.4987143834928,-0.776467051212444,
255.454553433309));
#15614=CARTESIAN_POINT('Ctrl Pts',(-13.4209962106934,1.954245477432,255.259551774659));
#15615=CARTESIAN_POINT('Ctrl Pts',(-14.7139269256754,5.73906412060058,255.064550116009));
#15616=CARTESIAN_POINT('Ctrl Pts',(-14.0731228766187,9.68696130320919,254.86954845736));
#15617=CARTESIAN_POINT('Ctrl Pts',(-11.6494430958588,12.868517261329,254.67454679871));
#15618=CARTESIAN_POINT('Ctrl Pts',(-8.01347384385351,14.5347254093925,254.47954514006));
#15619=CARTESIAN_POINT('Ctrl Pts',(-4.02120035240413,14.293324573354,254.28454348141));
#15620=CARTESIAN_POINT('Ctrl Pts',(-0.612489521633883,12.2011456932368,
254.089541822761));
#15621=CARTESIAN_POINT('Ctrl Pts',(1.41017492862557,8.75073259973012,253.894540164111));
#15622=CARTESIAN_POINT('Ctrl Pts',(1.57061435707062,4.7543866207135,253.699538505461));
#15623=CARTESIAN_POINT('Ctrl Pts',(-0.168942122637196,1.15293340734223,
253.504536846811));
#15624=CARTESIAN_POINT('Ctrl Pts',(-3.39896556422205,-1.20576762521993,
253.309535188161));
#15625=CARTESIAN_POINT('Ctrl Pts',(-7.35903909596598,-1.76642760896984,
253.114533529512));
#15626=CARTESIAN_POINT('Ctrl Pts',(-11.1168763796294,-0.397055145501226,
252.919531870862));
#15627=CARTESIAN_POINT('Ctrl Pts',(-13.7878018320942,2.57997008475345,252.724530212212));
#15628=CARTESIAN_POINT('Ctrl Pts',(-14.7430222529744,6.46379242128361,252.529528553562));
#15629=CARTESIAN_POINT('Ctrl Pts',(-13.7576582451438,10.3400766944335,252.334526894913));
#15630=CARTESIAN_POINT('Ctrl Pts',(-11.0636856533259,13.2962623565209,252.139525236263));
#15631=CARTESIAN_POINT('Ctrl Pts',(-7.29532346936788,14.6363998288394,251.944523577613));
#15632=CARTESIAN_POINT('Ctrl Pts',(-3.33972506390303,14.0449919755934,251.749521918963));
#15633=CARTESIAN_POINT('Ctrl Pts',(-0.128123234356899,11.6612689038728,
251.554520260313));
#15634=CARTESIAN_POINT('Ctrl Pts',(1.58340199056655,8.04641020695973,251.359518601664));
#15635=CARTESIAN_POINT('Ctrl Pts',(1.39192082384246,4.05143123868129,251.164516943014));
#15636=CARTESIAN_POINT('Ctrl Pts',(-0.657487956487292,0.616835826510511,
250.969515284364));
#15637=CARTESIAN_POINT('Ctrl Pts',(-4.08234951957581,-1.44879852348372,
250.774513625714));
#15638=CARTESIAN_POINT('Ctrl Pts',(-8.07637791642891,-1.65917713296756,
250.579511967064));
#15639=CARTESIAN_POINT('Ctrl Pts',(-11.6992931044972,0.0352276398836714,
250.384510308415));
#15640=CARTESIAN_POINT('Ctrl Pts',(-14.0981830589506,3.23551653006531,250.189508649765));
#15641=CARTESIAN_POINT('Ctrl Pts',(-14.7082975766551,7.18827281770608,249.994506991115));
#15642=CARTESIAN_POINT('Ctrl Pts',(-13.3860026000469,10.9629328009406,249.799505332465));
#15643=CARTESIAN_POINT('Ctrl Pts',(-10.4425947583245,13.670860471963,249.604503673815));
#15644=CARTESIAN_POINT('Ctrl Pts',(-6.57101545692357,14.6745515136434,249.409502015166));
#15645=CARTESIAN_POINT('Ctrl Pts',(-2.68271759214759,13.7377155039824,249.214500356516));
#15646=CARTESIAN_POINT('Ctrl Pts',(0.306910030888837,11.0809037549593,249.019498697866));
#15647=CARTESIAN_POINT('Ctrl Pts',(1.69404487785044,7.32958679813654,248.824497039216));
#15648=CARTESIAN_POINT('Ctrl Pts',(1.15212562178204,3.36690519167174,248.629495380566));
#15649=CARTESIAN_POINT('Ctrl Pts',(-1.19126830846199,0.125759270638291,
248.434493721917));
#15650=CARTESIAN_POINT('Ctrl Pts',(-4.78445166572806,-1.63081562286511,
248.239492063267));
#15651=CARTESIAN_POINT('Ctrl Pts',(-8.78151193590089,-1.48928404233019,
248.044490404617));
#15652=CARTESIAN_POINT('Ctrl Pts',(-12.2414553097526,0.517034438819197,
247.849488745967));
#15653=CARTESIAN_POINT('Ctrl Pts',(-14.3497368237319,3.91580937238954,247.654487087318));
#15654=CARTESIAN_POINT('Ctrl Pts',(-14.6100217480177,7.90689615989639,247.459485428668));
#15655=CARTESIAN_POINT('Ctrl Pts',(-12.9610334083361,11.5507072815698,247.264483770018));
#15656=CARTESIAN_POINT('Ctrl Pts',(-9.79097909742259,13.9894113507484,247.069482111368));
#15657=CARTESIAN_POINT('Ctrl Pts',(-5.84615759805796,14.648885089394,246.874480452718));
#15658=CARTESIAN_POINT('Ctrl Pts',(-2.0552647402959,13.3738741703752,246.679478794069));
#15659=CARTESIAN_POINT('Ctrl Pts',(0.689242221906646,10.4645436470296,246.484477135419));
#15660=CARTESIAN_POINT('Ctrl Pts',(1.74124672273713,6.6058121597596,246.289475476769));
#15661=CARTESIAN_POINT('Ctrl Pts',(0.853085831363201,2.70610845566047,246.094473818119));
#15662=CARTESIAN_POINT('Ctrl Pts',(-1.76615160827613,-0.316494584996361,
245.899472159469));
#15663=CARTESIAN_POINT('Ctrl Pts',(-5.49983370043381,-1.75040895297636,
245.70447050082));
#15664=CARTESIAN_POINT('Ctrl Pts',(-9.46898712215619,-1.25806570575758,
245.50946884217));
#15665=CARTESIAN_POINT('Ctrl Pts',(-12.7391541399936,1.04463785120515,245.31446718352));
#15666=CARTESIAN_POINT('Ctrl Pts',(-14.5405411877685,4.61556993669378,245.11946552487));
#15667=CARTESIAN_POINT('Ctrl Pts',(-14.4489041262702,8.61410440547796,244.924463866221));
#15668=CARTESIAN_POINT('Ctrl Pts',(-12.4861686596696,12.0987652958764,244.729462207571));
#15669=CARTESIAN_POINT('Ctrl Pts',(-9.11366086036101,14.2493724172449,244.534460548921));
#15670=CARTESIAN_POINT('Ctrl Pts',(-6.45596025354793,14.4556269470338,244.404459443155));
#15671=CARTESIAN_POINT('Ctrl Pts',(-5.18036787242628,14.2400462902765,244.339458890271));
#15672=CARTESIAN_POINT('Ctrl Pts',(-2.17696442109716,12.4936896459294,258.886209595194));
#15673=CARTESIAN_POINT('Ctrl Pts',(-1.18666420925076,11.7874603644412,258.82120904231));
#15674=CARTESIAN_POINT('Ctrl Pts',(0.440228799577828,9.88095277329113,258.691207936544));
#15675=CARTESIAN_POINT('Ctrl Pts',(1.24700262019175,6.20780816435965,258.496206277894));
#15676=CARTESIAN_POINT('Ctrl Pts',(0.229685845340515,2.58777411101262,258.301204619244));
#15677=CARTESIAN_POINT('Ctrl Pts',(-2.37185181727327,-0.127533036464177,
258.106202960595));
#15678=CARTESIAN_POINT('Ctrl Pts',(-5.94529650349566,-1.29854737465037,
257.911201301945));
#15679=CARTESIAN_POINT('Ctrl Pts',(-9.64930901441413,-0.649724643295287,
257.716199643295));
#15680=CARTESIAN_POINT('Ctrl Pts',(-12.6119171141539,1.66625481118851,257.521197984645));
#15681=CARTESIAN_POINT('Ctrl Pts',(-14.135644046359,5.10412998298705,257.326196325996));
#15682=CARTESIAN_POINT('Ctrl Pts',(-13.861778615253,8.85456514380678,257.131194667346));
#15683=CARTESIAN_POINT('Ctrl Pts',(-11.8547914355129,12.034620997221,256.936193008696));
#15684=CARTESIAN_POINT('Ctrl Pts',(-8.58717183770218,13.8956470450103,256.741191350046));
#15685=CARTESIAN_POINT('Ctrl Pts',(-4.82818696338679,13.9995164531848,256.546189691396));
#15686=CARTESIAN_POINT('Ctrl Pts',(-1.46278287172395,12.3217767520604,256.351188032747));
#15687=CARTESIAN_POINT('Ctrl Pts',(0.716752195883785,9.25740360642712,256.156186374097));
#15688=CARTESIAN_POINT('Ctrl Pts',(1.19730882121199,5.52781638254676,255.961184715447));
#15689=CARTESIAN_POINT('Ctrl Pts',(-0.134246313555596,2.01103993266644,
255.766183056797));
#15690=CARTESIAN_POINT('Ctrl Pts',(-2.96443655298958,-0.465001028602228,
255.571181398147));
#15691=CARTESIAN_POINT('Ctrl Pts',(-6.62697433982785,-1.31739330731701,
255.376179739498));
#15692=CARTESIAN_POINT('Ctrl Pts',(-10.2596196416587,-0.345465453031489,
255.181178080848));
#15693=CARTESIAN_POINT('Ctrl Pts',(-13.0071697546051,2.22196984587269,254.986176422198));
#15694=CARTESIAN_POINT('Ctrl Pts',(-14.2227923885739,5.78048319449142,254.791174763548));
#15695=CARTESIAN_POINT('Ctrl Pts',(-13.6203038739569,9.4923241432365,254.596173104898));
#15696=CARTESIAN_POINT('Ctrl Pts',(-11.3415429435809,12.4836456341042,254.401171446249));
#15697=CARTESIAN_POINT('Ctrl Pts',(-7.92297884889648,14.0502263597522,254.206169787599));
#15698=CARTESIAN_POINT('Ctrl Pts',(-4.16941497964704,13.8232595805219,254.011168128949));
#15699=CARTESIAN_POINT('Ctrl Pts',(-0.964520865428091,11.8561781495442,
253.816166470299));
#15700=CARTESIAN_POINT('Ctrl Pts',(0.937202605263502,8.61207527194551,253.62116481165));
#15701=CARTESIAN_POINT('Ctrl Pts',(1.088048894503,4.85468242098349,253.426163153));
#15702=CARTESIAN_POINT('Ctrl Pts',(-0.547494453099542,1.46857055077819,
253.23116149435));
#15703=CARTESIAN_POINT('Ctrl Pts',(-3.58438541588777,-0.749096899397535,
253.0361598357));
#15704=CARTESIAN_POINT('Ctrl Pts',(-7.3076746545037,-1.27623339504218,252.84115817705));
#15705=CARTESIAN_POINT('Ctrl Pts',(-10.8408199374328,0.0112603133497307,
252.646156518401));
#15706=CARTESIAN_POINT('Ctrl Pts',(-13.3520430030127,2.81028056235354,252.451154859751));
#15707=CARTESIAN_POINT('Ctrl Pts',(-14.2501480217857,6.46187788608574,252.256153201101));
#15708=CARTESIAN_POINT('Ctrl Pts',(-13.3237017886373,10.1063878691313,252.061151542451));
#15709=CARTESIAN_POINT('Ctrl Pts',(-10.7908096390754,12.8858146082488,251.866149883801));
#15710=CARTESIAN_POINT('Ctrl Pts',(-7.24776877019554,14.1458213704849,251.671148225152));
#15711=CARTESIAN_POINT('Ctrl Pts',(-3.52868707706655,13.5897755097268,251.476146566502));
#15712=CARTESIAN_POINT('Ctrl Pts',(-0.509116244652642,11.3485821607565,
251.281144907852));
#15713=CARTESIAN_POINT('Ctrl Pts',(1.10007191826787,7.94986635978842,251.086143249202));
#15714=CARTESIAN_POINT('Ctrl Pts',(0.920039966399679,4.19375878202392,250.891141590553));
#15715=CARTESIAN_POINT('Ctrl Pts',(-1.00682871322467,0.964527800673052,
250.696139931903));
#15716=CARTESIAN_POINT('Ctrl Pts',(-4.22690786058867,-0.977596274700365,
250.501138273253));
#15717=CARTESIAN_POINT('Ctrl Pts',(-7.98212170435301,-1.1753957363637,250.306136614603));
#15718=CARTESIAN_POINT('Ctrl Pts',(-11.388412275481,0.417695656017143,250.111134955953));
#15719=CARTESIAN_POINT('Ctrl Pts',(-13.6438656352338,3.42662998255425,249.916133297304));
#15720=CARTESIAN_POINT('Ctrl Pts',(-14.2174996346742,7.14303949633495,249.721131638654));
#15721=CARTESIAN_POINT('Ctrl Pts',(-12.9742685135307,10.6920016007892,249.526129980004));
#15722=CARTESIAN_POINT('Ctrl Pts',(-10.2068555718026,13.2380144148563,249.331128321354));
#15723=CARTESIAN_POINT('Ctrl Pts',(-6.56676923658599,14.1816918552946,249.136126662704));
#15724=CARTESIAN_POINT('Ctrl Pts',(-2.91096398943488,13.3008719904214,248.941125004055));
#15725=CARTESIAN_POINT('Ctrl Pts',(-0.100094881300308,10.8029187289803,
248.746123345405));
#15726=CARTESIAN_POINT('Ctrl Pts',(1.20409914610878,7.27590390362059,248.551121686755));
#15727=CARTESIAN_POINT('Ctrl Pts',(0.69458281563053,3.55016253464298,248.356120028105));
#15728=CARTESIAN_POINT('Ctrl Pts',(-1.50869278831339,0.502814137742552,
248.161118369455));
#15729=CARTESIAN_POINT('Ctrl Pts',(-4.88702928111861,-1.14873004328783,
247.966116710806));
#15730=CARTESIAN_POINT('Ctrl Pts',(-8.64509371369493,-1.0156610468397,247.771115052156));
#15731=CARTESIAN_POINT('Ctrl Pts',(-11.898157028509,0.870693827689635,247.576113393506));
#15732=CARTESIAN_POINT('Ctrl Pts',(-13.880378270122,4.06624614084761,247.381111734856));
#15733=CARTESIAN_POINT('Ctrl Pts',(-14.12510000314,7.81869426262842,247.186110076207));
#15734=CARTESIAN_POINT('Ctrl Pts',(-12.5747094635392,11.2446313388274,246.991108417557));
#15735=CARTESIAN_POINT('Ctrl Pts',(-9.59420190300037,13.5375182117999,246.796106758907));
#15736=CARTESIAN_POINT('Ctrl Pts',(-5.88525273346894,14.1575601010644,246.601105100257));
#15737=CARTESIAN_POINT('Ctrl Pts',(-2.3210283651816,12.9587857864344,246.406103441607));
#15738=CARTESIAN_POINT('Ctrl Pts',(0.259376558051009,10.2234125812861,246.211101782958));
#15739=CARTESIAN_POINT('Ctrl Pts',(1.24847865565592,6.59540585209445,246.016100124308));
#15740=CARTESIAN_POINT('Ctrl Pts',(0.413423482436507,2.92887675386613,245.821098465658));
#15741=CARTESIAN_POINT('Ctrl Pts',(-2.04920214666245,0.0870039240630693,
245.626096807008));
#15742=CARTESIAN_POINT('Ctrl Pts',(-5.55963654711201,-1.26117254099502,
245.431095148358));
#15743=CARTESIAN_POINT('Ctrl Pts',(-9.29146276272433,-0.798267925870965,
245.236093489709));
#15744=CARTESIAN_POINT('Ctrl Pts',(-12.3660970007984,1.36675030034017,245.041091831059));
#15745=CARTESIAN_POINT('Ctrl Pts',(-14.0597738873002,4.72416598950618,244.846090172409));
#15746=CARTESIAN_POINT('Ctrl Pts',(-13.9736160717445,8.48361647407905,244.651088513759));
#15747=CARTESIAN_POINT('Ctrl Pts',(-12.1282382567964,11.7599193733671,244.45608685511));
#15748=CARTESIAN_POINT('Ctrl Pts',(-8.95738248968529,13.781935451426,244.26108519646));
#15749=CARTESIAN_POINT('Ctrl Pts',(-6.45859351784204,13.9758574240922,244.131084090693));
#15750=CARTESIAN_POINT('Ctrl Pts',(-5.25927250841645,13.7731669606642,244.06608353781));
#15751=CARTESIAN_POINT('',(-5.02255860044588,15.1738049495011,244.886209595194));
#15752=CARTESIAN_POINT('Ctrl Pts',(-13.5606802741686,4.06871967504047,244.886209595194));
#15753=CARTESIAN_POINT('Ctrl Pts',(-13.6416999058547,4.25198474135208,244.886209595194));
#15754=CARTESIAN_POINT('Ctrl Pts',(-13.7151826312799,4.43828315373224,244.886209595194));
#15755=CARTESIAN_POINT('Ctrl Pts',(-13.7809288919042,4.62715219586253,244.886209595194));
#15756=CARTESIAN_POINT('Ctrl Pts',(-13.7981238459847,4.67654807748114,244.886209595194));
#15757=CARTESIAN_POINT('Ctrl Pts',(-13.8147894265217,4.72611998925969,244.886209595194));
#15758=CARTESIAN_POINT('Ctrl Pts',(-13.8309216335706,4.77586005181989,244.886209595194));
#15759=CARTESIAN_POINT('Ctrl Pts',(-13.8920913619837,4.96446326704244,244.886209595194));
#15760=CARTESIAN_POINT('Ctrl Pts',(-13.9455960634865,5.15548198727219,244.886209595194));
#15761=CARTESIAN_POINT('Ctrl Pts',(-13.9914834408764,5.34843841990208,244.886209595194));
#15762=CARTESIAN_POINT('Ctrl Pts',(-14.0221712830238,5.47748080329141,244.886209595194));
#15763=CARTESIAN_POINT('Ctrl Pts',(-14.0494513794723,5.60739045083055,244.886209595194));
#15764=CARTESIAN_POINT('Ctrl Pts',(-14.0733263319475,5.73803005416043,244.886209595194));
#15765=CARTESIAN_POINT('Ctrl Pts',(-14.0848264366772,5.80095663471375,244.886209595194));
#15766=CARTESIAN_POINT('Ctrl Pts',(-14.0955363513703,5.86405263259847,244.886209595194));
#15767=CARTESIAN_POINT('Ctrl Pts',(-14.1054555711143,5.92730296672008,244.886209595194));
#15768=CARTESIAN_POINT('Ctrl Pts',(-14.1099102436318,5.95570837887997,244.886209595194));
#15769=CARTESIAN_POINT('Ctrl Pts',(-14.114203857297,5.98413486412789,244.886209595194));
#15770=CARTESIAN_POINT('Ctrl Pts',(-14.1183365861332,6.01258036983195,244.886209595194));
#15771=CARTESIAN_POINT('Ctrl Pts',(-14.148435975581,6.21975398033503,244.886209595194));
#15772=CARTESIAN_POINT('Ctrl Pts',(-14.1700072218867,6.42794420942989,244.886209595194));
#15773=CARTESIAN_POINT('Ctrl Pts',(-14.183122304898,6.63659797625938,244.886209595194));
#15774=CARTESIAN_POINT('Ctrl Pts',(-14.1959167986966,6.84015134480945,244.886209595194));
#15775=CARTESIAN_POINT('Ctrl Pts',(-14.200663401768,7.04414668470632,244.886209595194));
#15776=CARTESIAN_POINT('Ctrl Pts',(-14.1973790954965,7.24809133966967,244.886209595194));
#15777=CARTESIAN_POINT('Ctrl Pts',(-14.1939713478628,7.45970129863671,244.886209595194));
#15778=CARTESIAN_POINT('Ctrl Pts',(-14.1819181544029,7.67125743925327,244.886209595194));
#15779=CARTESIAN_POINT('Ctrl Pts',(-14.1611803257851,7.88222052991278,244.886209595194));
#15780=CARTESIAN_POINT('Ctrl Pts',(-14.1585245428646,7.90923744587584,244.886209595194));
#15781=CARTESIAN_POINT('Ctrl Pts',(-14.1557261469623,7.93624508772895,244.886209595194));
#15782=CARTESIAN_POINT('Ctrl Pts',(-14.1527868126277,7.96322691161578,244.886209595194));
#15783=CARTESIAN_POINT('Ctrl Pts',(-14.1327741913593,8.14693415995982,244.886209595194));
#15784=CARTESIAN_POINT('Ctrl Pts',(-14.1062143898519,8.32961625926344,244.886209595194));
#15785=CARTESIAN_POINT('Ctrl Pts',(-14.0731550923849,8.51091582075917,244.886209595194));
#15786=CARTESIAN_POINT('Ctrl Pts',(-14.0365821385092,8.71148452633737,244.886209595194));
#15787=CARTESIAN_POINT('Ctrl Pts',(-13.9920559713202,8.91036170495516,244.886209595194));
#15788=CARTESIAN_POINT('Ctrl Pts',(-13.9398818306279,9.10715451221913,244.886209595194));
#15789=CARTESIAN_POINT('Ctrl Pts',(-13.8870437200209,9.30645171153857,244.886209595194));
#15790=CARTESIAN_POINT('Ctrl Pts',(-13.8263616491073,9.5036117606046,244.886209595194));
#15791=CARTESIAN_POINT('Ctrl Pts',(-13.7580989406148,9.69822902231716,244.886209595194));
#15792=CARTESIAN_POINT('Ctrl Pts',(-13.6893937488177,9.8941078057447,244.886209595194));
#15793=CARTESIAN_POINT('Ctrl Pts',(-13.613009170321,10.0874113903711,244.886209595194));
#15794=CARTESIAN_POINT('Ctrl Pts',(-13.5291615501821,10.2777189855474,244.886209595194));
#15795=CARTESIAN_POINT('Ctrl Pts',(-13.4588847736849,10.4372250551266,244.886209595194));
#15796=CARTESIAN_POINT('Ctrl Pts',(-13.3833642870213,10.5946265393459,244.886209595194));
#15797=CARTESIAN_POINT('Ctrl Pts',(-13.3027008011542,10.7496666223443,244.886209595194));
#15798=CARTESIAN_POINT('Ctrl Pts',(-13.2894851256601,10.7750679474108,244.886209595194));
#15799=CARTESIAN_POINT('Ctrl Pts',(-13.2761313475271,10.8004058623963,244.886209595194));
#15800=CARTESIAN_POINT('Ctrl Pts',(-13.2626398501178,10.8256792079891,244.886209595194));
#15801=CARTESIAN_POINT('Ctrl Pts',(-13.2511902780452,10.847127456697,244.886209595194));
#15802=CARTESIAN_POINT('Ctrl Pts',(-13.2396441383265,10.8685242469617,244.886209595194));
#15803=CARTESIAN_POINT('Ctrl Pts',(-13.228005484279,10.8898623047447,244.886209595194));
#15804=CARTESIAN_POINT('Ctrl Pts',(-13.1266071084601,11.0757639041474,244.886209595194));
#15805=CARTESIAN_POINT('Ctrl Pts',(-13.0181082120307,11.2573630403096,244.886209595194));
#15806=CARTESIAN_POINT('Ctrl Pts',(-12.9028146193286,11.4342494127783,244.886209595194));
#15807=CARTESIAN_POINT('Ctrl Pts',(-12.7863855232406,11.6128779035223,244.886209595194));
#15808=CARTESIAN_POINT('Ctrl Pts',(-12.6630270719645,11.7867010213949,244.886209595194));
#15809=CARTESIAN_POINT('Ctrl Pts',(-12.5330020233028,11.9552883416326,244.886209595194));
#15810=CARTESIAN_POINT('Ctrl Pts',(-12.5051012498885,11.9914638068286,244.886209595194));
#15811=CARTESIAN_POINT('Ctrl Pts',(-12.4768933316999,12.0273981416757,244.886209595194));
#15812=CARTESIAN_POINT('Ctrl Pts',(-12.4483805671437,12.063086999528,244.886209595194));
#15813=CARTESIAN_POINT('Ctrl Pts',(-12.3164995738421,12.2281598045195,244.886209595194));
#15814=CARTESIAN_POINT('Ctrl Pts',(-12.1781005112301,12.3879829814049,244.886209595194));
#15815=CARTESIAN_POINT('Ctrl Pts',(-12.033606732815,12.5423224318724,244.886209595194));
#15816=CARTESIAN_POINT('Ctrl Pts',(-11.8882086532915,12.6976278016873,244.886209595194));
#15817=CARTESIAN_POINT('Ctrl Pts',(-11.7366388964776,12.8473810885217,244.886209595194));
#15818=CARTESIAN_POINT('Ctrl Pts',(-11.5792852838968,12.9913137785295,244.886209595194));
#15819=CARTESIAN_POINT('Ctrl Pts',(-11.4919827660588,13.071170135373,244.886209595194));
#15820=CARTESIAN_POINT('Ctrl Pts',(-11.4028991143817,13.1492342086978,244.886209595194));
#15821=CARTESIAN_POINT('Ctrl Pts',(-11.3120956067516,13.2254553247554,244.886209595194));
#15822=CARTESIAN_POINT('Ctrl Pts',(-11.2929324571765,13.2415410100545,244.886209595194));
#15823=CARTESIAN_POINT('Ctrl Pts',(-11.2736926976274,13.2575446008321,244.886209595194));
#15824=CARTESIAN_POINT('Ctrl Pts',(-11.2543768861651,13.273465599029,244.886209595194));
#15825=CARTESIAN_POINT('Ctrl Pts',(-11.2343851389903,13.2899437351582,244.886209595194));
#15826=CARTESIAN_POINT('Ctrl Pts',(-11.214318599184,13.3063278760051,244.886209595194));
#15827=CARTESIAN_POINT('Ctrl Pts',(-11.1941818061718,13.3226146508888,244.886209595194));
#15828=CARTESIAN_POINT('Ctrl Pts',(-11.0256711873371,13.4589071833097,244.886209595194));
#15829=CARTESIAN_POINT('Ctrl Pts',(-10.85216239996,13.5884512574688,244.886209595194));
#15830=CARTESIAN_POINT('Ctrl Pts',(-10.6741349526739,13.7110348714328,244.886209595194));
#15831=CARTESIAN_POINT('Ctrl Pts',(-10.4945591404068,13.8346846365887,244.886209595194));
#15832=CARTESIAN_POINT('Ctrl Pts',(-10.3103852764165,13.9512528349893,244.886209595194));
#15833=CARTESIAN_POINT('Ctrl Pts',(-10.1220600987603,14.0604937305074,244.886209595194));
#15834=CARTESIAN_POINT('Ctrl Pts',(-9.9332803739495,14.1699982930447,244.886209595194));
#15835=CARTESIAN_POINT('Ctrl Pts',(-9.74032876130808,14.2721406262152,244.886209595194));
#15836=CARTESIAN_POINT('Ctrl Pts',(-9.54361713581158,14.3666376844702,244.886209595194));
#15837=CARTESIAN_POINT('Ctrl Pts',(-9.43177984793535,14.4203624944851,244.886209595194));
#15838=CARTESIAN_POINT('Ctrl Pts',(-9.31872655436916,14.4716154268187,244.886209595194));
#15839=CARTESIAN_POINT('Ctrl Pts',(-9.20452844087298,14.5203384387715,244.886209595194));
#15840=CARTESIAN_POINT('Ctrl Pts',(-9.04092708943691,14.5901395095377,244.886209595194));
#15841=CARTESIAN_POINT('Ctrl Pts',(-8.87497648096828,14.6547491997806,244.886209595194));
#15842=CARTESIAN_POINT('Ctrl Pts',(-8.70692766233866,14.7141407892771,244.886209595194));
#15843=CARTESIAN_POINT('Ctrl Pts',(-8.6334063041882,14.7401246096819,244.886209595194));
#15844=CARTESIAN_POINT('Ctrl Pts',(-8.55948320988161,14.7651093791428,244.886209595194));
#15845=CARTESIAN_POINT('Ctrl Pts',(-8.48517889259629,14.7890915593904,244.886209595194));
#15846=CARTESIAN_POINT('Ctrl Pts',(-8.44998101678734,14.8004518925826,244.886209595194));
#15847=CARTESIAN_POINT('Ctrl Pts',(-8.41469759425489,14.8115872424219,244.886209595194));
#15848=CARTESIAN_POINT('Ctrl Pts',(-8.37933078649837,14.8224971691949,244.886209595194));
#15849=CARTESIAN_POINT('Ctrl Pts',(-8.35485045205377,14.8300488447097,244.886209595194));
#15850=CARTESIAN_POINT('Ctrl Pts',(-8.33033806182638,14.8374900653625,244.886209595194));
#15851=CARTESIAN_POINT('Ctrl Pts',(-8.30579869883627,14.8448196425142,244.886209595194));
#15852=CARTESIAN_POINT('Ctrl Pts',(-8.09581085169372,14.9075401836779,244.886209595194));
#15853=CARTESIAN_POINT('Ctrl Pts',(-7.88375132882739,14.9621196129436,244.886209595194));
#15854=CARTESIAN_POINT('Ctrl Pts',(-7.67013298256505,15.0086098677565,244.886209595194));
#15855=CARTESIAN_POINT('Ctrl Pts',(-7.45228817486406,15.0560199371483,244.886209595194));
#15856=CARTESIAN_POINT('Ctrl Pts',(-7.23282171750465,15.0950178682759,244.886209595194));
#15857=CARTESIAN_POINT('Ctrl Pts',(-7.0122464777467,15.125614080605,244.886209595194));
#15858=CARTESIAN_POINT('Ctrl Pts',(-6.79076187738696,15.1563364312535,244.886209595194));
#15859=CARTESIAN_POINT('Ctrl Pts',(-6.56815868414206,15.1785878405488,244.886209595194));
#15860=CARTESIAN_POINT('Ctrl Pts',(-6.34493423868892,15.1923307336774,244.886209595194));
#15861=CARTESIAN_POINT('Ctrl Pts',(-6.12307246678007,15.20598973332,244.886209595194));
#15862=CARTESIAN_POINT('Ctrl Pts',(-5.90059633001586,15.2112438988409,244.886209595194));
#15863=CARTESIAN_POINT('Ctrl Pts',(-5.67798247999417,15.208006677574,244.886209595194));
#15864=CARTESIAN_POINT('Ctrl Pts',(-5.45949145586512,15.2048294098979,244.886209595194));
#15865=CARTESIAN_POINT('Ctrl Pts',(-5.24086713902449,15.1934723799368,244.886209595194));
#15866=CARTESIAN_POINT('Ctrl Pts',(-5.02255860044619,15.1738049495012,244.886209595194));
#15867=CARTESIAN_POINT('Ctrl Pts',(-2.5565939916359,-1.50913350781789,258.886209595194));
#15868=CARTESIAN_POINT('Ctrl Pts',(-2.36425176395604,-1.3944894355529,258.886209595194));
#15869=CARTESIAN_POINT('Ctrl Pts',(-2.1766718434797,-1.27277478699839,258.886209595194));
#15870=CARTESIAN_POINT('Ctrl Pts',(-1.99428412292338,-1.14416896494428,
258.886209595194));
#15871=CARTESIAN_POINT('Ctrl Pts',(-1.93366427166563,-1.10142449848557,
258.886209595194));
#15872=CARTESIAN_POINT('Ctrl Pts',(-1.87361822779059,-1.0579184173449,258.886209595194));
#15873=CARTESIAN_POINT('Ctrl Pts',(-1.81416252640475,-1.01365627442405,
258.886209595194));
#15874=CARTESIAN_POINT('Ctrl Pts',(-1.63480680238428,-0.88013386185092,
258.886209595194));
#15875=CARTESIAN_POINT('Ctrl Pts',(-1.4608203694423,-0.739733919894315,
258.886209595194));
#15876=CARTESIAN_POINT('Ctrl Pts',(-1.29251314946164,-0.592851231854552,
258.886209595194));
#15877=CARTESIAN_POINT('Ctrl Pts',(-1.12422973111361,-0.445989315637765,
258.886209595194));
#15878=CARTESIAN_POINT('Ctrl Pts',(-0.961623522417777,-0.29264590162531,
258.886209595194));
#15879=CARTESIAN_POINT('Ctrl Pts',(-0.805045885791296,-0.133184447506872,
258.886209595194));
#15880=CARTESIAN_POINT('Ctrl Pts',(-0.649718484741496,0.0250037444309419,
258.886209595194));
#15881=CARTESIAN_POINT('Ctrl Pts',(-0.500323440890837,0.189213250571515,
258.886209595194));
#15882=CARTESIAN_POINT('Ctrl Pts',(-0.357249980777704,0.359111132088609,
258.886209595194));
#15883=CARTESIAN_POINT('Ctrl Pts',(-0.29718860122125,0.430433242699247,
258.886209595194));
#15884=CARTESIAN_POINT('Ctrl Pts',(-0.238241845667419,0.50275801433704,
258.886209595194));
#15885=CARTESIAN_POINT('Ctrl Pts',(-0.180441176696654,0.576061603721381,
258.886209595194));
#15886=CARTESIAN_POINT('Ctrl Pts',(-0.144784954550875,0.621281306429199,
258.886209595194));
#15887=CARTESIAN_POINT('Ctrl Pts',(-0.109564900728486,0.666873500247899,
258.886209595194));
#15888=CARTESIAN_POINT('Ctrl Pts',(-0.0747887191667214,0.712832650035259,
258.886209595194));
#15889=CARTESIAN_POINT('Ctrl Pts',(-0.0563480485347127,0.73720328262615,
258.886209595194));
#15890=CARTESIAN_POINT('Ctrl Pts',(-0.038030742298959,0.761679150596887,
258.886209595194));
#15891=CARTESIAN_POINT('Ctrl Pts',(-0.0198518056549546,0.78624046597595,
258.886209595194));
#15892=CARTESIAN_POINT('Ctrl Pts',(0.110489913750218,0.9623433998302,258.886209595194));
#15893=CARTESIAN_POINT('Ctrl Pts',(0.233876948226976,1.14303894425533,258.886209595194));
#15894=CARTESIAN_POINT('Ctrl Pts',(0.35002118159745,1.32795518664564,258.886209595194));
#15895=CARTESIAN_POINT('Ctrl Pts',(0.465425226174361,1.51169295528488,258.886209595194));
#15896=CARTESIAN_POINT('Ctrl Pts',(0.573678798737716,1.69959838513866,258.886209595194));
#15897=CARTESIAN_POINT('Ctrl Pts',(0.674454146436358,1.89133064568259,258.886209595194));
#15898=CARTESIAN_POINT('Ctrl Pts',(0.734138634723959,2.00488462609662,258.886209595194));
#15899=CARTESIAN_POINT('Ctrl Pts',(0.791199155867516,2.11978133151867,258.886209595194));
#15900=CARTESIAN_POINT('Ctrl Pts',(0.84555942095047,2.23595271429465,258.886209595194));
#15901=CARTESIAN_POINT('Ctrl Pts',(0.937957038195646,2.43341236509285,258.886209595194));
#15902=CARTESIAN_POINT('Ctrl Pts',(1.02255618128302,2.63455462652551,258.886209595194));
#15903=CARTESIAN_POINT('Ctrl Pts',(1.09921502593214,2.83889578394013,258.886209595194));
#15904=CARTESIAN_POINT('Ctrl Pts',(1.17522871899264,3.04151723082521,258.886209595194));
#15905=CARTESIAN_POINT('Ctrl Pts',(1.24343521127095,3.24728464096187,258.886209595194));
#15906=CARTESIAN_POINT('Ctrl Pts',(1.30364535510154,3.45572494737603,258.886209595194));
#15907=CARTESIAN_POINT('Ctrl Pts',(1.32167511638107,3.51814182145381,258.886209595194));
#15908=CARTESIAN_POINT('Ctrl Pts',(1.33898750665215,3.58079832257484,258.886209595194));
#15909=CARTESIAN_POINT('Ctrl Pts',(1.35557654598764,3.64368158286573,258.886209595194));
#15910=CARTESIAN_POINT('Ctrl Pts',(1.36363610324781,3.67423255250119,258.886209595194));
#15911=CARTESIAN_POINT('Ctrl Pts',(1.37152572241146,3.70484048731049,258.886209595194));
#15912=CARTESIAN_POINT('Ctrl Pts',(1.37923843311511,3.73547835131255,258.886209595194));
#15913=CARTESIAN_POINT('Ctrl Pts',(1.43147363965295,3.94297675434062,258.886209595194));
#15914=CARTESIAN_POINT('Ctrl Pts',(1.47566023134054,4.15207335701424,258.886209595194));
#15915=CARTESIAN_POINT('Ctrl Pts',(1.51173350642158,4.36229864068028,258.886209595194));
#15916=CARTESIAN_POINT('Ctrl Pts',(1.54773548735025,4.57210844132261,258.886209595194));
#15917=CARTESIAN_POINT('Ctrl Pts',(1.57565622252453,4.78304316299326,258.886209595194));
#15918=CARTESIAN_POINT('Ctrl Pts',(1.59537984651403,4.99464074758762,258.886209595194));
#15919=CARTESIAN_POINT('Ctrl Pts',(1.6148216062332,5.20321445589954,258.886209595194));
#15920=CARTESIAN_POINT('Ctrl Pts',(1.62629879805449,5.41243284840401,258.886209595194));
#15921=CARTESIAN_POINT('Ctrl Pts',(1.62965074073741,5.62184810818147,258.886209595194));
#15922=CARTESIAN_POINT('Ctrl Pts',(1.6327194156952,5.8135659936726,258.886209595194));
#15923=CARTESIAN_POINT('Ctrl Pts',(1.62897759367094,6.00544917304189,258.886209595194));
#15924=CARTESIAN_POINT('Ctrl Pts',(1.61826513272597,6.19714342809054,258.886209595194));
#15925=CARTESIAN_POINT('Ctrl Pts',(1.60917103257037,6.35987790746193,258.886209595194));
#15926=CARTESIAN_POINT('Ctrl Pts',(1.59505249145376,6.5224762007389,258.886209595194));
#15927=CARTESIAN_POINT('Ctrl Pts',(1.57593654055478,6.68470751761093,258.886209595194));
#15928=CARTESIAN_POINT('Ctrl Pts',(1.5719647517677,6.71841489260214,258.886209595194));
#15929=CARTESIAN_POINT('Ctrl Pts',(1.56777717341846,6.75210639050512,258.886209595194));
#15930=CARTESIAN_POINT('Ctrl Pts',(1.56337396690442,6.78577988384794,258.886209595194));
#15931=CARTESIAN_POINT('Ctrl Pts',(1.5587180818881,6.82138573440307,258.886209595194));
#15932=CARTESIAN_POINT('Ctrl Pts',(1.55382011111554,6.85697788318115,258.886209595194));
#15933=CARTESIAN_POINT('Ctrl Pts',(1.54868546689053,6.89251890151437,258.886209595194));
#15934=CARTESIAN_POINT('Ctrl Pts',(1.51896610042817,7.09823063187067,258.886209595194));
#15935=CARTESIAN_POINT('Ctrl Pts',(1.48130244852888,7.30240357228093,258.886209595194));
#15936=CARTESIAN_POINT('Ctrl Pts',(1.43587337478814,7.50459721844464,258.886209595194));
#15937=CARTESIAN_POINT('Ctrl Pts',(1.38852851662937,7.71531755038135,258.886209595194));
#15938=CARTESIAN_POINT('Ctrl Pts',(1.33274952436721,7.92388900443129,258.886209595194));
#15939=CARTESIAN_POINT('Ctrl Pts',(1.26868210430257,8.12979485754507,258.886209595194));
#15940=CARTESIAN_POINT('Ctrl Pts',(1.20747747983608,8.3264999910211,258.886209595194));
#15941=CARTESIAN_POINT('Ctrl Pts',(1.13870795870331,8.5207728894651,258.886209595194));
#15942=CARTESIAN_POINT('Ctrl Pts',(1.06245554283562,8.71213744821539,258.886209595194));
#15943=CARTESIAN_POINT('Ctrl Pts',(0.987089797793576,8.9012768004673,258.886209595194));
#15944=CARTESIAN_POINT('Ctrl Pts',(0.904413843326177,9.08757558348147,258.886209595194));
#15945=CARTESIAN_POINT('Ctrl Pts',(0.814468490237699,9.2705410852132,258.886209595194));
#15946=CARTESIAN_POINT('Ctrl Pts',(0.762052691576746,9.3771645245724,258.886209595194));
#15947=CARTESIAN_POINT('Ctrl Pts',(0.707167515950218,9.4826553245914,258.886209595194));
#15948=CARTESIAN_POINT('Ctrl Pts',(0.649815571343313,9.58690963773167,258.886209595194));
#15949=CARTESIAN_POINT('Ctrl Pts',(0.628692976237029,9.6253062720505,258.886209595194));
#15950=CARTESIAN_POINT('Ctrl Pts',(0.607235742908852,9.66353513548064,258.886209595194));
#15951=CARTESIAN_POINT('Ctrl Pts',(0.585443872533378,9.70159086009454,258.886209595194));
#15952=CARTESIAN_POINT('Ctrl Pts',(0.569448520810109,9.72952396954294,258.886209595194));
#15953=CARTESIAN_POINT('Ctrl Pts',(0.55327160296368,9.75736582506558,258.886209595194));
#15954=CARTESIAN_POINT('Ctrl Pts',(0.536925022550999,9.78509443608612,258.886209595194));
#15955=CARTESIAN_POINT('Ctrl Pts',(0.515073579604955,9.82216091399109,258.886209595194));
#15956=CARTESIAN_POINT('Ctrl Pts',(0.492914635658092,9.85903272341201,258.886209595194));
#15957=CARTESIAN_POINT('Ctrl Pts',(0.470449172522589,9.89570560295486,258.886209595194));
#15958=CARTESIAN_POINT('Ctrl Pts',(0.363857027480884,10.0697078423812,258.886209595194));
#15959=CARTESIAN_POINT('Ctrl Pts',(0.250367525613926,10.2392345429506,258.886209595194));
#15960=CARTESIAN_POINT('Ctrl Pts',(0.130333176594055,10.4039506937353,258.886209595194));
#15961=CARTESIAN_POINT('Ctrl Pts',(0.0103337666115684,10.5686188997126,
258.886209595194));
#15962=CARTESIAN_POINT('Ctrl Pts',(-0.116207256219615,10.7284798091608,
258.886209595194));
#15963=CARTESIAN_POINT('Ctrl Pts',(-0.248971466524913,10.8831592822246,
258.886209595194));
#15964=CARTESIAN_POINT('Ctrl Pts',(-0.317445405170305,10.9629361492275,
258.886209595194));
#15965=CARTESIAN_POINT('Ctrl Pts',(-0.387575234292688,11.0413340485417,
258.886209595194));
#15966=CARTESIAN_POINT('Ctrl Pts',(-0.459320022478923,11.1182969478255,
258.886209595194));
#15967=CARTESIAN_POINT('Ctrl Pts',(-0.515939682919651,11.1790346450735,
258.886209595194));
#15968=CARTESIAN_POINT('Ctrl Pts',(-0.573565190357813,11.2388785523942,
258.886209595194));
#15969=CARTESIAN_POINT('Ctrl Pts',(-0.632177086784188,11.2977995896963,
258.886209595194));
#15970=CARTESIAN_POINT('Ctrl Pts',(-0.650664912710916,11.3163849272724,
258.886209595194));
#15971=CARTESIAN_POINT('Ctrl Pts',(-0.669248914573616,11.3348764140862,
258.886209595194));
#15972=CARTESIAN_POINT('Ctrl Pts',(-0.687922396772642,11.3532673475919,
258.886209595194));
#15973=CARTESIAN_POINT('Ctrl Pts',(-0.830665427309727,11.4938505315441,
258.886209595194));
#15974=CARTESIAN_POINT('Ctrl Pts',(-0.978735934932914,11.6286636650011,
258.886209595194));
#15975=CARTESIAN_POINT('Ctrl Pts',(-1.13181485672381,11.7573645070508,258.886209595194));
#15976=CARTESIAN_POINT('Ctrl Pts',(-1.2837913086776,11.885138449468,258.886209595194));
#15977=CARTESIAN_POINT('Ctrl Pts',(-1.44070486494264,12.0068881819309,258.886209595194));
#15978=CARTESIAN_POINT('Ctrl Pts',(-1.60226714821513,12.1222335635334,258.886209595194));
#15979=CARTESIAN_POINT('Ctrl Pts',(-1.76109169330005,12.2356243710263,258.886209595194));
#15980=CARTESIAN_POINT('Ctrl Pts',(-1.92440928861502,12.3428262801963,258.886209595194));
#15981=CARTESIAN_POINT('Ctrl Pts',(-2.09196087277376,12.4434299668365,258.886209595194));
#15982=CARTESIAN_POINT('Ctrl Pts',(-2.120175705855,12.4603711150815,258.886209595194));
#15983=CARTESIAN_POINT('Ctrl Pts',(-2.14851062563325,12.4771250413085,258.886209595194));
#15984=CARTESIAN_POINT('Ctrl Pts',(-2.17696442109716,12.4936896459294,258.886209595194));
#15985=CARTESIAN_POINT('Ctrl Pts',(-5.02255860044619,15.1738049495012,244.886209595194));
#15986=CARTESIAN_POINT('Ctrl Pts',(-6.45069372495988,15.415165992917,244.951210148077));
#15987=CARTESIAN_POINT('Ctrl Pts',(-7.93845566333615,15.2997061708998,245.01621070096));
#15988=CARTESIAN_POINT('Ctrl Pts',(-9.3116386098082,14.84067805856,245.081211253844));
#15989=CARTESIAN_POINT('Ctrl Pts',(-10.6848215562803,14.3816499462201,245.146211806727));
#15990=CARTESIAN_POINT('Ctrl Pts',(-11.9434255108482,13.5790535435577,245.21121235961));
#15991=CARTESIAN_POINT('Ctrl Pts',(-12.9389692831164,12.5275258634565,245.276212912493));
#15992=CARTESIAN_POINT('Ctrl Pts',(-13.9345130553847,11.4759981833554,245.341213465377));
#15993=CARTESIAN_POINT('Ctrl Pts',(-14.6669966453531,10.1755392258155,245.40621401826));
#15994=CARTESIAN_POINT('Ctrl Pts',(-15.0503376992346,8.77919267417778,245.471214571143));
#15995=CARTESIAN_POINT('Ctrl Pts',(-15.259915832765,8.01578969114034,245.506751319461));
#15996=CARTESIAN_POINT('Ctrl Pts',(-15.365136378047,7.22372621266417,245.542288067779));
#15997=CARTESIAN_POINT('Ctrl Pts',(-15.3653307732302,6.43170986456378,245.577824816097));
#15998=CARTESIAN_POINT('Origin',(-6.5,6.43177298256785,244.886209595194));
#15999=CARTESIAN_POINT('',(-17.5,6.43177298256785,244.886209595194));
#16000=CARTESIAN_POINT('Origin',(-6.5,6.43177298256785,244.886209595194));
#16001=CARTESIAN_POINT('Origin',(-6.5,6.43177298256785,244.886209595194));
#16002=CARTESIAN_POINT('Origin',(-6.5,6.43177298256785,260.886209595194));
#16003=CARTESIAN_POINT('',(-17.5,6.43177298256785,236.886209595194));
#16004=CARTESIAN_POINT('Origin',(-6.5,6.43177298256785,236.886209595194));
#16005=CARTESIAN_POINT('',(-17.5,6.43177298256785,260.886209595194));
#16006=CARTESIAN_POINT('Origin',(-6.5,6.43177298256785,236.886209595194));
#16007=CARTESIAN_POINT('',(-13.5,6.43177298256785,236.886209595194));
#16008=CARTESIAN_POINT('Origin',(-6.5,6.43177298256785,236.886209595194));
#16009=CARTESIAN_POINT('Origin',(-6.5,6.43177298256785,258.886209595194));
#16010=CARTESIAN_POINT('',(-13.5,6.43177298256785,258.886209595194));
#16011=CARTESIAN_POINT('Origin',(-6.5,6.43177298256785,258.886209595194));
#16012=CARTESIAN_POINT('Origin',(-6.5,6.43177298256785,260.886209595194));
#16013=CARTESIAN_POINT('',(-13.5,6.43177298256785,260.886209595194));
#16014=CARTESIAN_POINT('Origin',(-6.5,6.43177298256785,260.886209595194));
#16015=CARTESIAN_POINT('',(0.,0.,0.));
#16016=CARTESIAN_POINT('Ctrl Pts',(-14.7402854682776,21.6688065021356,-26.5483789742253));
#16017=CARTESIAN_POINT('Ctrl Pts',(-14.7402854682776,21.6688065021356,-26.6605787118535));
#16018=CARTESIAN_POINT('Ctrl Pts',(-14.7220127764577,21.5774430430356,-26.9228448679022));
#16019=CARTESIAN_POINT('Ctrl Pts',(-14.6702053983118,21.3184061523065,-27.0483789742253));
#16020=CARTESIAN_POINT('Ctrl Pts',(-14.6402854682776,21.1688065021356,-27.0483789742253));
#16021=CARTESIAN_POINT('Ctrl Pts',(-14.8450052233973,21.6688065021356,-26.5483789742253));
#16022=CARTESIAN_POINT('Ctrl Pts',(-14.8450052233973,21.6688065021356,-26.6843099042658));
#16023=CARTESIAN_POINT('Ctrl Pts',(-14.779646000333,21.5310977797265,-26.9707326579855));
#16024=CARTESIAN_POINT('Ctrl Pts',(-14.6901520183346,21.2984595322837,-27.0483789742253));
#16025=CARTESIAN_POINT('Ctrl Pts',(-14.6402854682776,21.1688065021356,-27.0483789742253));
#16026=CARTESIAN_POINT('Ctrl Pts',(-15.0535348863446,21.5820559202025,-26.5483789742253));
#16027=CARTESIAN_POINT('Ctrl Pts',(-15.0535348863446,21.5820559202025,-26.7112475141754));
#16028=CARTESIAN_POINT('Ctrl Pts',(-14.8957223019916,21.4242433358495,-27.0209351418812));
#16029=CARTESIAN_POINT('Ctrl Pts',(-14.7300452583802,21.2585662922382,-27.0483789742253));
#16030=CARTESIAN_POINT('Ctrl Pts',(-14.6402854682776,21.1688065021356,-27.0483789742253));
#16031=CARTESIAN_POINT('Ctrl Pts',(-15.1402854682776,21.3735262572552,-26.5483789742253));
#16032=CARTESIAN_POINT('Ctrl Pts',(-15.1402854682776,21.3735262572552,-26.6843099042658));
#16033=CARTESIAN_POINT('Ctrl Pts',(-15.0025767458686,21.308167034191,-26.9707326579855));
#16034=CARTESIAN_POINT('Ctrl Pts',(-14.7699384984258,21.2186730521926,-27.0483789742253));
#16035=CARTESIAN_POINT('Ctrl Pts',(-14.6402854682776,21.1688065021356,-27.0483789742253));
#16036=CARTESIAN_POINT('Ctrl Pts',(-15.1402854682776,21.2688065021356,-26.5483789742253));
#16037=CARTESIAN_POINT('Ctrl Pts',(-15.1402854682776,21.2688065021356,-26.6605787118535));
#16038=CARTESIAN_POINT('Ctrl Pts',(-15.0489220091777,21.2505338103156,-26.9228448679022));
#16039=CARTESIAN_POINT('Ctrl Pts',(-14.7898851184486,21.1987264321698,-27.0483789742253));
#16040=CARTESIAN_POINT('Ctrl Pts',(-14.6402854682776,21.1688065021356,-27.0483789742253));
#16041=CARTESIAN_POINT('',(-14.7402854682776,21.6688065021356,-26.5483789742253));
#16042=CARTESIAN_POINT('',(-14.6402854682776,21.1688065021356,-27.0483789742253));
#16043=CARTESIAN_POINT('Origin',(-14.6402854682776,21.1688065021356,-26.5483789742253));
#16044=CARTESIAN_POINT('',(-15.1402854682776,21.2688065021356,-26.5483789742253));
#16045=CARTESIAN_POINT('Origin',(-14.6402854682776,21.1688065021356,-26.5483789742253));
#16046=CARTESIAN_POINT('Origin',(-14.7402854682776,21.2688065021356,-26.5483789742253));
#16047=CARTESIAN_POINT('Ctrl Pts',(-15.1402854682776,17.8031073387245,-26.5483789742253));
#16048=CARTESIAN_POINT('Ctrl Pts',(-15.1402854682776,17.8031073387245,-26.6605787118535));
#16049=CARTESIAN_POINT('Ctrl Pts',(-15.048928983054,17.8213786357693,-26.9228506801488));
#16050=CARTESIAN_POINT('Ctrl Pts',(-14.7898851184486,17.8731874086903,-27.0483789742253));
#16051=CARTESIAN_POINT('Ctrl Pts',(-14.6402854682776,17.9031073387245,-27.0483789742253));
#16052=CARTESIAN_POINT('Ctrl Pts',(-15.1402854682776,17.6983875836049,-26.5483789742253));
#16053=CARTESIAN_POINT('Ctrl Pts',(-15.1402854682776,17.6983875836049,-26.6843099042658));
#16054=CARTESIAN_POINT('Ctrl Pts',(-15.0025886096795,17.7637448778075,-26.9707646203248));
#16055=CARTESIAN_POINT('Ctrl Pts',(-14.7699384984258,17.8532407886675,-27.0483789742253));
#16056=CARTESIAN_POINT('Ctrl Pts',(-14.6402854682776,17.9031073387245,-27.0483789742253));
#16057=CARTESIAN_POINT('Ctrl Pts',(-15.0535392142239,17.4898535927783,-26.5483789742253));
#16058=CARTESIAN_POINT('Ctrl Pts',(-15.0535392142239,17.4898535927783,-26.7112475141754));
#16059=CARTESIAN_POINT('Ctrl Pts',(-14.8957171704612,17.647675636541,-27.0210148571608));
#16060=CARTESIAN_POINT('Ctrl Pts',(-14.7300452583802,17.813347548622,-27.0483789742253));
#16061=CARTESIAN_POINT('Ctrl Pts',(-14.6402854682777,17.9031073387245,-27.0483789742253));
#16062=CARTESIAN_POINT('Ctrl Pts',(-14.8450052233973,17.4031073387245,-26.5483789742253));
#16063=CARTESIAN_POINT('Ctrl Pts',(-14.8450052233973,17.4031073387245,-26.6843099042658));
#16064=CARTESIAN_POINT('Ctrl Pts',(-14.7796479291947,17.5408041973226,-26.9707646203248));
#16065=CARTESIAN_POINT('Ctrl Pts',(-14.6901520183346,17.7734543085764,-27.0483789742253));
#16066=CARTESIAN_POINT('Ctrl Pts',(-14.6402854682776,17.9031073387245,-27.0483789742253));
#16067=CARTESIAN_POINT('Ctrl Pts',(-14.7402854682776,17.4031073387245,-26.5483789742253));
#16068=CARTESIAN_POINT('Ctrl Pts',(-14.7402854682776,17.4031073387245,-26.6605787118535));
#16069=CARTESIAN_POINT('Ctrl Pts',(-14.7220141712329,17.4944638239482,-26.9228506801488));
#16070=CARTESIAN_POINT('Ctrl Pts',(-14.6702053983118,17.7535076885536,-27.0483789742253));
#16071=CARTESIAN_POINT('Ctrl Pts',(-14.6402854682776,17.9031073387245,-27.0483789742253));
#16072=CARTESIAN_POINT('',(-15.1402854682776,17.8031073387245,-26.5483789742253));
#16073=CARTESIAN_POINT('',(-14.6402854682776,17.9031073387245,-27.0483789742253));
#16074=CARTESIAN_POINT('Origin',(-14.6402854682776,17.9031073387245,-26.5483789742253));
#16075=CARTESIAN_POINT('',(-14.7402854682776,17.4031073387245,-26.5483789742253));
#16076=CARTESIAN_POINT('Origin',(-14.6402854682776,17.9031073387245,-26.5483789742253));
#16077=CARTESIAN_POINT('Origin',(-14.7402854682776,17.8031073387245,-26.5483789742253));
#16078=CARTESIAN_POINT('Ctrl Pts',(1.74028546827765,17.4031073387245,-26.5483789742253));
#16079=CARTESIAN_POINT('Ctrl Pts',(1.74028546827765,17.4031073387245,-26.6605787118535));
#16080=CARTESIAN_POINT('Ctrl Pts',(1.72202043385628,17.4944325108313,-26.9228767774799));
#16081=CARTESIAN_POINT('Ctrl Pts',(1.67020539831183,17.7535076885536,-27.0483789742253));
#16082=CARTESIAN_POINT('Ctrl Pts',(1.64028546827764,17.9031073387245,-27.0483789742253));
#16083=CARTESIAN_POINT('Ctrl Pts',(1.84500522339731,17.4031073387245,-26.5483789742253));
#16084=CARTESIAN_POINT('Ctrl Pts',(1.84500522339731,17.4031073387245,-26.6843099042658));
#16085=CARTESIAN_POINT('Ctrl Pts',(1.77965658989769,17.5407509281098,-26.970908133119));
#16086=CARTESIAN_POINT('Ctrl Pts',(1.69015201833462,17.7734543085764,-27.0483789742253));
#16087=CARTESIAN_POINT('Ctrl Pts',(1.64028546827764,17.9031073387245,-27.0483789742253));
#16088=CARTESIAN_POINT('Ctrl Pts',(2.05355924307323,17.4898335639289,-26.5483789742253));
#16089=CARTESIAN_POINT('Ctrl Pts',(2.05355924307323,17.4898335639289,-26.7112475141754));
#16090=CARTESIAN_POINT('Ctrl Pts',(1.8956931882834,17.6476996187188,-27.0213738612389));
#16091=CARTESIAN_POINT('Ctrl Pts',(1.73004525838021,17.813347548622,-27.0483789742253));
#16092=CARTESIAN_POINT('Ctrl Pts',(1.64028546827764,17.9031073387245,-27.0483789742253));
#16093=CARTESIAN_POINT('Ctrl Pts',(2.14028546827764,17.6983875836049,-26.5483789742253));
#16094=CARTESIAN_POINT('Ctrl Pts',(2.14028546827764,17.6983875836049,-26.6843099042658));
#16095=CARTESIAN_POINT('Ctrl Pts',(2.00264187889234,17.7637362171045,-26.970908133119));
#16096=CARTESIAN_POINT('Ctrl Pts',(1.76993849842579,17.8532407886675,-27.0483789742253));
#16097=CARTESIAN_POINT('Ctrl Pts',(1.64028546827764,17.9031073387245,-27.0483789742253));
#16098=CARTESIAN_POINT('Ctrl Pts',(2.14028546827764,17.8031073387245,-26.5483789742253));
#16099=CARTESIAN_POINT('Ctrl Pts',(2.14028546827764,17.8031073387245,-26.6605787118535));
#16100=CARTESIAN_POINT('Ctrl Pts',(2.04896029617083,17.8213723731459,-26.9228767774799));
#16101=CARTESIAN_POINT('Ctrl Pts',(1.78988511844858,17.8731874086903,-27.0483789742253));
#16102=CARTESIAN_POINT('Ctrl Pts',(1.64028546827764,17.9031073387245,-27.0483789742253));
#16103=CARTESIAN_POINT('',(1.74028546827765,17.4031073387245,-26.5483789742253));
#16104=CARTESIAN_POINT('',(1.64028546827764,17.9031073387245,-27.0483789742253));
#16105=CARTESIAN_POINT('Origin',(1.64028546827764,17.9031073387245,-26.5483789742253));
#16106=CARTESIAN_POINT('',(2.14028546827764,17.8031073387245,-26.5483789742253));
#16107=CARTESIAN_POINT('Origin',(1.64028546827764,17.9031073387245,-26.5483789742253));
#16108=CARTESIAN_POINT('Origin',(1.74028546827765,17.8031073387245,-26.5483789742253));
#16109=CARTESIAN_POINT('Ctrl Pts',(2.14028546827765,21.2688065021356,-26.5483789742253));
#16110=CARTESIAN_POINT('Ctrl Pts',(2.14028546827765,21.2688065021356,-26.6605787118535));
#16111=CARTESIAN_POINT('Ctrl Pts',(2.04895072597714,21.2505395536755,-26.9228688013811));
#16112=CARTESIAN_POINT('Ctrl Pts',(1.78988511844859,21.1987264321698,-27.0483789742253));
#16113=CARTESIAN_POINT('Ctrl Pts',(1.64028546827765,21.1688065021356,-27.0483789742253));
#16114=CARTESIAN_POINT('Ctrl Pts',(2.14028546827765,21.3735262572552,-26.5483789742253));
#16115=CARTESIAN_POINT('Ctrl Pts',(2.14028546827765,21.3735262572552,-26.6843099042658));
#16116=CARTESIAN_POINT('Ctrl Pts',(2.00262559828104,21.3081749767944,-26.9708642714605));
#16117=CARTESIAN_POINT('Ctrl Pts',(1.7699384984258,21.2186730521926,-27.0483789742253));
#16118=CARTESIAN_POINT('Ctrl Pts',(1.64028546827765,21.1688065021356,-27.0483789742253));
#16119=CARTESIAN_POINT('Ctrl Pts',(2.05355301579653,21.5820740496545,-26.5483789742253));
#16120=CARTESIAN_POINT('Ctrl Pts',(2.05355301579653,21.5820740496545,-26.7112475141754));
#16121=CARTESIAN_POINT('Ctrl Pts',(1.8957006850393,21.4242217188972,-27.0212639478808));
#16122=CARTESIAN_POINT('Ctrl Pts',(1.73004525838021,21.2585662922381,-27.0483789742253));
#16123=CARTESIAN_POINT('Ctrl Pts',(1.64028546827765,21.1688065021356,-27.0483789742253));
#16124=CARTESIAN_POINT('Ctrl Pts',(1.84500522339731,21.6688065021356,-26.5483789742253));
#16125=CARTESIAN_POINT('Ctrl Pts',(1.84500522339731,21.6688065021356,-26.6843099042658));
#16126=CARTESIAN_POINT('Ctrl Pts',(1.7796539429365,21.531146632139,-26.9708642714605));
#16127=CARTESIAN_POINT('Ctrl Pts',(1.69015201833463,21.2984595322837,-27.0483789742253));
#16128=CARTESIAN_POINT('Ctrl Pts',(1.64028546827765,21.1688065021356,-27.0483789742253));
#16129=CARTESIAN_POINT('Ctrl Pts',(1.74028546827765,21.6688065021356,-26.5483789742253));
#16130=CARTESIAN_POINT('Ctrl Pts',(1.74028546827765,21.6688065021356,-26.6605787118535));
#16131=CARTESIAN_POINT('Ctrl Pts',(1.72201851981755,21.5774717598351,-26.9228688013811));
#16132=CARTESIAN_POINT('Ctrl Pts',(1.67020539831184,21.3184061523065,-27.0483789742253));
#16133=CARTESIAN_POINT('Ctrl Pts',(1.64028546827765,21.1688065021356,-27.0483789742253));
#16134=CARTESIAN_POINT('',(2.14028546827765,21.2688065021356,-26.5483789742253));
#16135=CARTESIAN_POINT('',(1.64028546827765,21.1688065021356,-27.0483789742253));
#16136=CARTESIAN_POINT('Origin',(1.64028546827765,21.1688065021356,-26.5483789742253));
#16137=CARTESIAN_POINT('',(1.74028546827765,21.6688065021356,-26.5483789742253));
#16138=CARTESIAN_POINT('Origin',(1.64028546827765,21.1688065021356,-26.5483789742253));
#16139=CARTESIAN_POINT('Origin',(1.74028546827765,21.2688065021356,-26.5483789742253));
#16140=CARTESIAN_POINT('Origin',(-10.6201427341388,21.1688065021356,-26.5483789742253));
#16141=CARTESIAN_POINT('',(-10.6201427341388,21.6688065021356,-26.5483789742253));
#16142=CARTESIAN_POINT('',(-10.6201427341388,21.1688065021356,-27.0483789742253));
#16143=CARTESIAN_POINT('Origin',(1.64028546827765,20.4023817112828,-26.5483789742253));
#16144=CARTESIAN_POINT('',(1.64028546827765,20.4023817112828,-27.0483789742253));
#16145=CARTESIAN_POINT('',(2.14028546827765,20.4023817112828,-26.5483789742253));
#16146=CARTESIAN_POINT('Origin',(-2.37985726586118,17.9031073387245,-26.5483789742253));
#16147=CARTESIAN_POINT('',(-2.37985726586118,17.9031073387245,-27.0483789742253));
#16148=CARTESIAN_POINT('',(-2.37985726586118,17.4031073387245,-26.5483789742253));
#16149=CARTESIAN_POINT('Origin',(-14.6402854682776,18.6695321295773,-26.5483789742253));
#16150=CARTESIAN_POINT('',(-14.6402854682776,18.6695321295773,-27.0483789742253));
#16151=CARTESIAN_POINT('',(-15.1402854682776,18.6695321295773,-26.5483789742253));
#16152=CARTESIAN_POINT('Origin',(1.74028546827765,17.4031073387245,-25.0483789742253));
#16153=CARTESIAN_POINT('',(1.74028546827765,17.4031073387245,-19.0483789742253));
#16154=CARTESIAN_POINT('',(1.74028546827765,17.4031073387245,-25.0483789742253));
#16155=CARTESIAN_POINT('',(-14.7402854682776,17.4031073387245,-19.0483789742253));
#16156=CARTESIAN_POINT('',(-2.37985726586118,17.4031073387245,-19.0483789742253));
#16157=CARTESIAN_POINT('',(-14.7402854682776,17.4031073387245,-25.0483789742253));
#16158=CARTESIAN_POINT('Origin',(1.74028546827765,17.8031073387245,-25.0483789742253));
#16159=CARTESIAN_POINT('',(2.14028546827764,17.8031073387245,-19.0483789742253));
#16160=CARTESIAN_POINT('',(2.14028546827764,17.8031073387245,-25.0483789742253));
#16161=CARTESIAN_POINT('Origin',(1.74028546827765,17.8031073387245,-19.0483789742253));
#16162=CARTESIAN_POINT('Origin',(2.14028546827765,21.2688065021356,-25.0483789742253));
#16163=CARTESIAN_POINT('',(2.14028546827765,21.2688065021356,-19.0483789742253));
#16164=CARTESIAN_POINT('',(2.14028546827765,21.2688065021356,-25.0483789742253));
#16165=CARTESIAN_POINT('',(2.14028546827765,20.4023817112828,-19.0483789742253));
#16166=CARTESIAN_POINT('Origin',(1.74028546827765,21.2688065021356,-25.0483789742253));
#16167=CARTESIAN_POINT('',(1.74028546827764,21.6688065021356,-19.0483789742253));
#16168=CARTESIAN_POINT('',(1.74028546827764,21.6688065021356,-25.0483789742253));
#16169=CARTESIAN_POINT('Origin',(1.74028546827765,21.2688065021356,-19.0483789742253));
#16170=CARTESIAN_POINT('Origin',(-6.5,19.5359569204301,-27.0483789742253));
#16171=CARTESIAN_POINT('',(-8.88488236958947,19.6738537403084,-27.0483789742253));
#16172=CARTESIAN_POINT('',(-11.4348823695895,19.6738537403084,-27.0483789742253));
#16173=CARTESIAN_POINT('Origin',(-10.1598823695895,19.4201314511811,-27.0483789742253));
#16174=CARTESIAN_POINT('',(-11.4348823695895,19.1664091620538,-27.0483789742253));
#16175=CARTESIAN_POINT('Origin',(-12.7098823695895,19.4201314511811,-27.0483789742253));
#16176=CARTESIAN_POINT('',(-8.88488236958947,19.1664091620538,-27.0483789742253));
#16177=CARTESIAN_POINT('Origin',(-10.1598823695895,19.4201314511811,-27.0483789742253));
#16178=CARTESIAN_POINT('Origin',(-7.60988236958947,19.4201314511811,-27.0483789742253));
#16179=CARTESIAN_POINT('Origin',(1.74028546827765,23.2688065021356,-25.0483789742253));
#16180=CARTESIAN_POINT('',(1.74028546827765,23.2688065021356,-19.0483789742253));
#16181=CARTESIAN_POINT('',(-14.7402854682776,23.2688065021356,-19.0483789742253));
#16182=CARTESIAN_POINT('',(-2.37985726586118,23.2688065021356,-19.0483789742253));
#16183=CARTESIAN_POINT('',(-14.7402854682776,23.2688065021356,-17.8483789742253));
#16184=CARTESIAN_POINT('',(-14.7402854682776,23.2688065021356,-25.0483789742253));
#16185=CARTESIAN_POINT('',(1.74028546827765,23.2688065021356,-17.8483789742253));
#16186=CARTESIAN_POINT('',(-14.7402854682776,23.2688065021356,-17.8483789742253));
#16187=CARTESIAN_POINT('',(1.74028546827765,23.2688065021356,-25.0483789742253));
#16188=CARTESIAN_POINT('Origin',(-14.7402854682776,21.2688065021356,-25.0483789742253));
#16189=CARTESIAN_POINT('',(-16.7402854682776,21.2688065021356,-19.0483789742253));
#16190=CARTESIAN_POINT('Origin',(-14.7402854682776,21.2688065021356,-19.0483789742253));
#16191=CARTESIAN_POINT('',(-16.7402854682776,21.2688065021356,-17.8483789742253));
#16192=CARTESIAN_POINT('',(-16.7402854682776,21.2688065021356,-25.0483789742253));
#16193=CARTESIAN_POINT('Origin',(-14.7402854682776,21.2688065021356,-17.8483789742253));
#16194=CARTESIAN_POINT('Origin',(-16.7402854682776,21.2688065021356,-25.0483789742253));
#16195=CARTESIAN_POINT('',(-16.7402854682776,17.8031073387245,-19.0483789742253));
#16196=CARTESIAN_POINT('',(-16.7402854682776,20.4023817112828,-19.0483789742253));
#16197=CARTESIAN_POINT('',(-16.7402854682776,17.8031073387245,-17.8483789742253));
#16198=CARTESIAN_POINT('',(-16.7402854682776,17.8031073387245,-25.0483789742253));
#16199=CARTESIAN_POINT('',(-16.7402854682776,17.8031073387245,-17.8483789742253));
#16200=CARTESIAN_POINT('Origin',(-14.7402854682776,17.8031073387245,-25.0483789742253));
#16201=CARTESIAN_POINT('',(-14.7402854682776,15.8031073387245,-19.0483789742253));
#16202=CARTESIAN_POINT('Origin',(-14.7402854682776,17.8031073387245,-19.0483789742253));
#16203=CARTESIAN_POINT('',(-14.7402854682776,15.8031073387245,-17.8483789742253));
#16204=CARTESIAN_POINT('',(-14.7402854682776,15.8031073387245,-25.0483789742253));
#16205=CARTESIAN_POINT('Origin',(-14.7402854682776,17.8031073387245,-17.8483789742253));
#16206=CARTESIAN_POINT('Origin',(1.74028546827765,21.2688065021356,-25.0483789742253));
#16207=CARTESIAN_POINT('',(3.74028546827765,21.2688065021356,-19.0483789742253));
#16208=CARTESIAN_POINT('Origin',(1.74028546827765,21.2688065021356,-19.0483789742253));
#16209=CARTESIAN_POINT('',(3.74028546827765,21.2688065021356,-17.8483789742253));
#16210=CARTESIAN_POINT('Origin',(1.74028546827765,21.2688065021356,-17.8483789742253));
#16211=CARTESIAN_POINT('',(3.74028546827765,21.2688065021356,-25.0483789742253));
#16212=CARTESIAN_POINT('Origin',(3.74028546827765,17.8031073387245,-25.0483789742253));
#16213=CARTESIAN_POINT('',(3.74028546827765,17.8031073387245,-19.0483789742253));
#16214=CARTESIAN_POINT('',(3.74028546827765,18.6695321295773,-19.0483789742253));
#16215=CARTESIAN_POINT('',(3.74028546827765,17.8031073387245,-17.8483789742253));
#16216=CARTESIAN_POINT('',(3.74028546827765,21.2688065021356,-17.8483789742253));
#16217=CARTESIAN_POINT('',(3.74028546827765,17.8031073387245,-25.0483789742253));
#16218=CARTESIAN_POINT('Origin',(1.74028546827765,17.8031073387245,-25.0483789742253));
#16219=CARTESIAN_POINT('',(1.74028546827765,15.8031073387245,-19.0483789742253));
#16220=CARTESIAN_POINT('Origin',(1.74028546827765,17.8031073387245,-19.0483789742253));
#16221=CARTESIAN_POINT('',(1.74028546827765,15.8031073387245,-17.8483789742253));
#16222=CARTESIAN_POINT('Origin',(1.74028546827765,17.8031073387245,-17.8483789742253));
#16223=CARTESIAN_POINT('',(1.74028546827764,15.8031073387245,-25.0483789742253));
#16224=CARTESIAN_POINT('Origin',(-14.7402854682776,15.8031073387245,-25.0483789742253));
#16225=CARTESIAN_POINT('',(-10.6201427341388,15.8031073387245,-19.0483789742253));
#16226=CARTESIAN_POINT('',(1.74028546827764,15.8031073387245,-17.8483789742253));
#16227=CARTESIAN_POINT('Origin',(-6.5,19.5359569204301,-17.8483789742253));
#16228=CARTESIAN_POINT('',(-11.4348823695895,19.6738537403084,-17.8483789742253));
#16229=CARTESIAN_POINT('',(-8.88488236958947,19.6738537403084,-17.8483789742253));
#16230=CARTESIAN_POINT('Origin',(-10.1598823695895,19.4201314511811,-17.8483789742253));
#16231=CARTESIAN_POINT('',(-8.88488236958947,19.1664091620538,-17.8483789742253));
#16232=CARTESIAN_POINT('Origin',(-7.60988236958947,19.4201314511811,-17.8483789742253));
#16233=CARTESIAN_POINT('',(-11.4348823695895,19.1664091620538,-17.8483789742253));
#16234=CARTESIAN_POINT('Origin',(-10.1598823695895,19.4201314511811,-17.8483789742253));
#16235=CARTESIAN_POINT('Origin',(-12.7098823695895,19.4201314511811,-17.8483789742253));
#16236=CARTESIAN_POINT('Origin',(-6.5,19.5359569204301,-19.0483789742253));
#16237=CARTESIAN_POINT('',(-15.1402854682776,17.8031073387245,-19.0483789742253));
#16238=CARTESIAN_POINT('',(-15.1402854682776,21.2688065021356,-19.0483789742253));
#16239=CARTESIAN_POINT('',(-15.1402854682776,18.6695321295773,-19.0483789742253));
#16240=CARTESIAN_POINT('Origin',(-14.7402854682776,17.8031073387245,-19.0483789742253));
#16241=CARTESIAN_POINT('',(-14.7402854682776,21.6688065021356,-19.0483789742253));
#16242=CARTESIAN_POINT('',(-10.6201427341388,21.6688065021356,-19.0483789742253));
#16243=CARTESIAN_POINT('Origin',(-14.7402854682776,21.2688065021356,-19.0483789742253));
#16244=CARTESIAN_POINT('Origin',(-7.60988236958947,19.4201314511811,-25.0483789742253));
#16245=CARTESIAN_POINT('',(-8.88488236958947,19.6738537403084,-25.0483789742253));
#16246=CARTESIAN_POINT('',(-8.88488236958947,19.1664091620538,-25.0483789742253));
#16247=CARTESIAN_POINT('Origin',(-10.1598823695895,19.4201314511811,-25.0483789742253));
#16248=CARTESIAN_POINT('',(-11.4348823695895,19.1664091620538,-25.0483789742253));
#16249=CARTESIAN_POINT('Origin',(-12.7098823695895,19.4201314511811,-25.0483789742253));
#16250=CARTESIAN_POINT('',(-11.4348823695895,19.6738537403084,-25.0483789742253));
#16251=CARTESIAN_POINT('Origin',(-10.1598823695895,19.4201314511811,-25.0483789742253));
#16252=CARTESIAN_POINT('Origin',(-15.1402854682776,17.8031073387245,-25.0483789742253));
#16253=CARTESIAN_POINT('',(-15.1402854682776,17.8031073387245,-25.0483789742253));
#16254=CARTESIAN_POINT('',(-15.1402854682776,21.2688065021356,-25.0483789742253));
#16255=CARTESIAN_POINT('Origin',(-14.7402854682776,17.8031073387245,-25.0483789742253));
#16256=CARTESIAN_POINT('Origin',(-14.7402854682776,21.6688065021356,-25.0483789742253));
#16257=CARTESIAN_POINT('',(-14.7402854682776,21.6688065021356,-25.0483789742253));
#16258=CARTESIAN_POINT('Origin',(-14.7402854682776,21.2688065021356,-25.0483789742253));
#16259=CARTESIAN_POINT('',(0.,0.,0.));
#16260=CARTESIAN_POINT('Origin',(-0.744000000195138,0.744000000196221,1.2));
#16261=CARTESIAN_POINT('',(-0.744000000195138,0.248000000196221,1.15122809938326));
#16262=CARTESIAN_POINT('',(-0.248000000195138,0.744000000196666,1.15122809938313));
#16263=CARTESIAN_POINT('Ctrl Pts',(-0.744000000195138,0.248000000196221,
1.15122809938326));
#16264=CARTESIAN_POINT('Ctrl Pts',(-0.743548129195526,0.248000000196221,
1.15128162561029));
#16265=CARTESIAN_POINT('Ctrl Pts',(-0.743096462399636,0.248000617700407,
1.15133505381795));
#16266=CARTESIAN_POINT('Ctrl Pts',(-0.68084251616827,0.248170686680912,
1.1586889909138));
#16267=CARTESIAN_POINT('Ctrl Pts',(-0.614748859330863,0.260619583354249,
1.16502989619583));
#16268=CARTESIAN_POINT('Ctrl Pts',(-0.492966510303847,0.311166686726808,
1.17344391775669));
#16269=CARTESIAN_POINT('Ctrl Pts',(-0.437280006866291,0.349270066587974,
1.17551763482271));
#16270=CARTESIAN_POINT('Ctrl Pts',(-0.393275036726453,0.393275036727851,
1.17551763482269));
#16271=CARTESIAN_POINT('Ctrl Pts',(-0.349270066586615,0.437280006867729,
1.17551763482268));
#16272=CARTESIAN_POINT('Ctrl Pts',(-0.3111666867255,0.49296651030532,1.17344391775664));
#16273=CARTESIAN_POINT('Ctrl Pts',(-0.26061958335305,0.61474885933238,1.16502989619573));
#16274=CARTESIAN_POINT('Ctrl Pts',(-0.248170686679772,0.680842516169798,
1.15868899091368));
#16275=CARTESIAN_POINT('Ctrl Pts',(-0.248000617699323,0.743096462401038,
1.15133505381783));
#16276=CARTESIAN_POINT('Ctrl Pts',(-0.248000000195138,0.743548129196929,
1.15128162561017));
#16277=CARTESIAN_POINT('Ctrl Pts',(-0.248000000195138,0.744000000196666,
1.15122809938313));
#16278=CARTESIAN_POINT('',(-0.744000000195138,0.248000000196221,0.583389912843141));
#16279=CARTESIAN_POINT('',(-0.744000000195138,0.248000000196221,1.2));
#16280=CARTESIAN_POINT('',(-0.516876228118667,0.303056928861888,0.19));
#16281=CARTESIAN_POINT('Origin',(-0.744000000195138,0.744000000196221,0.583389912843142));
#16282=CARTESIAN_POINT('',(-0.303056928861701,0.51687622811801,0.19));
#16283=CARTESIAN_POINT('Origin',(-0.744000000195138,0.744000000196221,0.19));
#16284=CARTESIAN_POINT('',(-0.248000000195138,0.744000000196666,0.583389912846777));
#16285=CARTESIAN_POINT('Origin',(-0.744000000195138,0.744000000196221,0.583389912847341));
#16286=CARTESIAN_POINT('',(-0.248000000195138,0.744000000196666,1.2));
#16287=CARTESIAN_POINT('Origin',(-0.248000000194694,0.24800000019315,1.2));
#16288=CARTESIAN_POINT('',(-0.24800000019541,1.04682989872245,1.10790668314437));
#16289=CARTESIAN_POINT('Origin',(-0.248000000194471,-2.22346593631069E-13,
-5.12965591734105));
#16290=CARTESIAN_POINT('',(-0.248000000195362,0.993500000023809,1.01553658903582));
#16291=CARTESIAN_POINT('Origin',(-0.248000000195457,1.09999999999962,1.2));
#16292=CARTESIAN_POINT('',(0.248000000196041,1.04682989872314,1.10790668314423));
#16293=CARTESIAN_POINT('Origin',(2.9811416492917E-12,-1.91582141081592,
-4.02355591008723));
#16294=CARTESIAN_POINT('',(0.303056928861511,0.516876228118951,0.19));
#16295=CARTESIAN_POINT('',(-0.124000000097707,0.516876228118288,0.19));
#16296=CARTESIAN_POINT('',(0.248000000196085,0.744000000194883,0.583389912842355));
#16297=CARTESIAN_POINT('Origin',(0.744000000196085,0.744000000194955,0.583389912841147));
#16298=CARTESIAN_POINT('',(0.248000000196033,1.1000000000003,1.19999999999985));
#16299=CARTESIAN_POINT('Origin',(0.248000000196033,1.10000000000039,1.2));
#16300=CARTESIAN_POINT('',(0.248000000196085,0.744000000194883,1.1512280993833));
#16301=CARTESIAN_POINT('Origin',(0.248000000196193,3.61135222251268E-14,
-5.12965591734105));
#16302=CARTESIAN_POINT('',(0.248000000196085,0.744000000194883,1.2));
#16303=CARTESIAN_POINT('Origin',(0.744000000196085,0.744000000194955,1.2));
#16304=CARTESIAN_POINT('',(0.744000000196732,0.248000000194955,1.15122809938313));
#16305=CARTESIAN_POINT('Ctrl Pts',(0.248000000196085,0.744000000194883,
1.1512280993833));
#16306=CARTESIAN_POINT('Ctrl Pts',(0.248000000196085,0.743548129195249,
1.15128162561033));
#16307=CARTESIAN_POINT('Ctrl Pts',(0.24800061770027,0.743096462399337,1.15133505381799));
#16308=CARTESIAN_POINT('Ctrl Pts',(0.248170686680793,0.68084251616795,1.15868899091384));
#16309=CARTESIAN_POINT('Ctrl Pts',(0.260619583354148,0.614748859330546,
1.16502989619587));
#16310=CARTESIAN_POINT('Ctrl Pts',(0.311166686726741,0.492966510303544,
1.17344391775672));
#16311=CARTESIAN_POINT('Ctrl Pts',(0.349270066587923,0.437280006865998,
1.17551763482273));
#16312=CARTESIAN_POINT('Ctrl Pts',(0.393275036727812,0.393275036726173,
1.17551763482271));
#16313=CARTESIAN_POINT('Ctrl Pts',(0.437280006867702,0.349270066586347,
1.1755176348227));
#16314=CARTESIAN_POINT('Ctrl Pts',(0.492966510305304,0.311166686725247,
1.17344391775665));
#16315=CARTESIAN_POINT('Ctrl Pts',(0.614748859332378,0.26061958335283,1.16502989619575));
#16316=CARTESIAN_POINT('Ctrl Pts',(0.6808425161698,0.248170686679572,1.15868899091369));
#16317=CARTESIAN_POINT('Ctrl Pts',(0.743096462401062,0.24800061769914,1.15133505381783));
#16318=CARTESIAN_POINT('Ctrl Pts',(0.743548129196974,0.248000000194955,
1.15128162561017));
#16319=CARTESIAN_POINT('Ctrl Pts',(0.744000000196732,0.248000000194955,
1.15122809938313));
#16320=CARTESIAN_POINT('',(0.516876228118432,0.30305692886123,0.19));
#16321=CARTESIAN_POINT('Origin',(0.744000000196085,0.744000000194955,0.19));
#16322=CARTESIAN_POINT('',(0.744000000196732,0.248000000194955,0.583389912846289));
#16323=CARTESIAN_POINT('Origin',(0.744000000196085,0.744000000194955,0.583389912845349));
#16324=CARTESIAN_POINT('',(0.744000000196732,0.248000000194955,1.2));
#16325=CARTESIAN_POINT('Origin',(0.248000000196157,0.248000000194308,1.2));
#16326=CARTESIAN_POINT('',(1.04682989872277,0.24800000019535,1.10790668314432));
#16327=CARTESIAN_POINT('Origin',(-3.16340915708764E-13,0.248000000193984,
-5.12965591734105));
#16328=CARTESIAN_POINT('',(0.99350000002449,0.248000000195281,1.01553658903639));
#16329=CARTESIAN_POINT('Origin',(1.09999999999997,0.248000000195419,1.2));
#16330=CARTESIAN_POINT('',(1.04682989872287,-0.248000000195507,1.1079066831443));
#16331=CARTESIAN_POINT('Origin',(-1.91582141081591,-4.04170800382928E-13,
-4.02355591008723));
#16332=CARTESIAN_POINT('',(0.51687622811856,-0.3030569288607,0.19));
#16333=CARTESIAN_POINT('',(0.51687622811847,0.124000000097702,0.19));
#16334=CARTESIAN_POINT('',(0.744000000195517,-0.248000000195115,0.583389912844004));
#16335=CARTESIAN_POINT('Origin',(0.744000000194874,-0.744000000195115,0.583389912842708));
#16336=CARTESIAN_POINT('',(1.09999999999998,-0.248000000195576,1.19999999999984));
#16337=CARTESIAN_POINT('Origin',(1.10000000000007,-0.248000000195576,1.2));
#16338=CARTESIAN_POINT('',(0.744000000195517,-0.248000000195115,1.15122809938326));
#16339=CARTESIAN_POINT('Origin',(-3.14351440352569E-13,-0.24800000019415,
-5.12965591734105));
#16340=CARTESIAN_POINT('',(0.744000000195517,-0.248000000195115,1.2));
#16341=CARTESIAN_POINT('Origin',(-0.744000000195415,-0.744000000194864,
1.2));
#16342=CARTESIAN_POINT('',(-0.248000000195415,-0.744000000196249,1.15122809938316));
#16343=CARTESIAN_POINT('',(-0.744000000196312,-0.248000000194864,1.15122809938318));
#16344=CARTESIAN_POINT('Ctrl Pts',(-0.248000000195415,-0.744000000196249,
1.15122809938316));
#16345=CARTESIAN_POINT('Ctrl Pts',(-0.248000000195414,-0.74354812919633,
1.15128162561023));
#16346=CARTESIAN_POINT('Ctrl Pts',(-0.248000617699598,-0.743096462400134,
1.15133505381792));
#16347=CARTESIAN_POINT('Ctrl Pts',(-0.248170686680046,-0.680842516168463,
1.15868899091381));
#16348=CARTESIAN_POINT('Ctrl Pts',(-0.260619583353321,-0.614748859331044,
1.16502989619585));
#16349=CARTESIAN_POINT('Ctrl Pts',(-0.311166686725766,-0.49296651030398,
1.17344391775673));
#16350=CARTESIAN_POINT('Ctrl Pts',(-0.349270066586879,-0.437280006866388,
1.17551763482276));
#16351=CARTESIAN_POINT('Ctrl Pts',(-0.393275036726715,-0.393275036726509,
1.17551763482276));
#16352=CARTESIAN_POINT('Ctrl Pts',(-0.437280006866551,-0.349270066586629,
1.17551763482276));
#16353=CARTESIAN_POINT('Ctrl Pts',(-0.492966510304106,-0.311166686725461,
1.17344391775673));
#16354=CARTESIAN_POINT('Ctrl Pts',(-0.61474885933112,-0.260619583352896,
1.16502989619586));
#16355=CARTESIAN_POINT('Ctrl Pts',(-0.680842516168527,-0.248170686679557,
1.15868899091382));
#16356=CARTESIAN_POINT('Ctrl Pts',(-0.743096462400073,-0.248000617699049,
1.15133505381795));
#16357=CARTESIAN_POINT('Ctrl Pts',(-0.74354812919627,-0.248000000194863,
1.15128162561025));
#16358=CARTESIAN_POINT('Ctrl Pts',(-0.744000000196312,-0.248000000194864,
1.15122809938318));
#16359=CARTESIAN_POINT('',(-0.248000000195415,-0.744000000196249,0.58338991284606));
#16360=CARTESIAN_POINT('',(-0.248000000195415,-0.744000000196249,1.2));
#16361=CARTESIAN_POINT('',(-0.303056928861281,-0.516876228118006,0.19));
#16362=CARTESIAN_POINT('Origin',(-0.744000000195415,-0.744000000194864,
0.583389912845007));
#16363=CARTESIAN_POINT('',(-0.516876228118667,-0.303056928860673,0.19));
#16364=CARTESIAN_POINT('Origin',(-0.744000000195415,-0.744000000194864,
0.19));
#16365=CARTESIAN_POINT('',(-0.744000000196312,-0.248000000194864,0.583389912845176));
#16366=CARTESIAN_POINT('Origin',(-0.744000000195415,-0.744000000194864,
0.583389912843621));
#16367=CARTESIAN_POINT('',(-0.744000000196312,-0.248000000194864,1.2));
#16368=CARTESIAN_POINT('Origin',(-0.24800000019403,-0.248000000193966,1.2));
#16369=CARTESIAN_POINT('',(-1.04682989872298,-0.248000000195412,1.10790668314428));
#16370=CARTESIAN_POINT('Origin',(4.5589868649524E-13,-0.248000000193518,
-5.12965591734105));
#16371=CARTESIAN_POINT('',(-0.993500000024419,-0.248000000195315,1.01553658903588));
#16372=CARTESIAN_POINT('Origin',(0.744000000194874,-0.744000000195115,1.2));
#16373=CARTESIAN_POINT('',(0.248000000194874,-0.744000000196067,1.15122809938321));
#16374=CARTESIAN_POINT('Ctrl Pts',(0.744000000195517,-0.248000000195115,
1.15122809938326));
#16375=CARTESIAN_POINT('Ctrl Pts',(0.743548129195714,-0.248000000195114,
1.15128162561031));
#16376=CARTESIAN_POINT('Ctrl Pts',(0.743096462399633,-0.248000617699299,
1.15133505381799));
#16377=CARTESIAN_POINT('Ctrl Pts',(0.680842516168076,-0.248170686679796,
1.15868899091386));
#16378=CARTESIAN_POINT('Ctrl Pts',(0.614748859330666,-0.260619583353124,
1.1650298961959));
#16379=CARTESIAN_POINT('Ctrl Pts',(0.492966510303643,-0.311166686725667,
1.17344391775676));
#16380=CARTESIAN_POINT('Ctrl Pts',(0.437280006866081,-0.349270066586825,
1.17551763482279));
#16381=CARTESIAN_POINT('Ctrl Pts',(0.393275036726237,-0.393275036726696,
1.17551763482278));
#16382=CARTESIAN_POINT('Ctrl Pts',(0.349270066586393,-0.437280006866568,
1.17551763482278));
#16383=CARTESIAN_POINT('Ctrl Pts',(0.31116668672527,-0.492966510304154,
1.17344391775674));
#16384=CARTESIAN_POINT('Ctrl Pts',(0.260619583352803,-0.614748859331208,
1.16502989619586));
#16385=CARTESIAN_POINT('Ctrl Pts',(0.248170686679517,-0.680842516168625,
1.15868899091381));
#16386=CARTESIAN_POINT('Ctrl Pts',(0.248000617699059,-0.743096462400057,
1.15133505381795));
#16387=CARTESIAN_POINT('Ctrl Pts',(0.248000000194873,-0.743548129196139,
1.15128162561027));
#16388=CARTESIAN_POINT('Ctrl Pts',(0.248000000194874,-0.744000000196067,
1.15122809938321));
#16389=CARTESIAN_POINT('',(0.30305692886038,-0.516876228118955,0.19));
#16390=CARTESIAN_POINT('Origin',(0.744000000194874,-0.744000000195115,0.19));
#16391=CARTESIAN_POINT('',(0.248000000194874,-0.744000000196067,0.5833899128444));
#16392=CARTESIAN_POINT('Origin',(0.744000000194874,-0.744000000195115,0.583389912841405));
#16393=CARTESIAN_POINT('',(0.248000000194874,-0.744000000196067,1.2));
#16394=CARTESIAN_POINT('Origin',(0.248000000193922,-0.248000000194471,1.2));
#16395=CARTESIAN_POINT('',(0.248000000195456,-1.04682989872316,1.10790668314425));
#16396=CARTESIAN_POINT('Origin',(0.248000000193446,4.75999652275667E-13,
-5.12965591734105));
#16397=CARTESIAN_POINT('',(0.248000000195353,-0.993500000024651,1.01553658903593));
#16398=CARTESIAN_POINT('Origin',(-1.10000000000019,0.248000000196221,1.2));
#16399=CARTESIAN_POINT('',(-1.04682989872296,0.248000000196221,1.10790668314426));
#16400=CARTESIAN_POINT('Origin',(7.17605422133295E-15,0.248000000196221,
-5.12965591734105));
#16401=CARTESIAN_POINT('',(-1.10000000000019,0.248000000196221,1.2));
#16402=CARTESIAN_POINT('Origin',(-1.10000000000019,-0.248000000195508,1.2));
#16403=CARTESIAN_POINT('',(-1.04942373620595,-1.28517341949389E-16,1.11239934145138));
#16404=CARTESIAN_POINT('Origin',(1.91582141081578,-5.36035544273609E-16,
-4.02355591008731));
#16405=CARTESIAN_POINT('',(-0.516876228118667,-0.124000000097755,0.19));
#16406=CARTESIAN_POINT('Origin',(1.91582141081578,-5.36035544273609E-16,
-4.02355591008731));
#16407=CARTESIAN_POINT('Origin',(-0.248000000196409,-1.09999999999961,1.2));
#16408=CARTESIAN_POINT('',(-0.24800000019626,-1.04682989872243,1.10790668314434));
#16409=CARTESIAN_POINT('Origin',(-0.248000000193338,6.92337424395539E-13,
-5.12965591734105));
#16410=CARTESIAN_POINT('',(-0.248000000196409,-1.09999999999954,1.19999999999987));
#16411=CARTESIAN_POINT('Origin',(0.248000000195558,-1.10000000000039,1.2));
#16412=CARTESIAN_POINT('Origin',(3.00794342650252E-12,1.91582141081592,
-4.02355591008723));
#16413=CARTESIAN_POINT('',(0.124000000097801,-0.516876228118675,0.19));
#16414=CARTESIAN_POINT('Origin',(-5.91193760612896E-14,-1.66533453693773E-15,
0.19));
#16415=CARTESIAN_POINT('Origin',(0.,0.,-0.1));
#16416=CARTESIAN_POINT('',(0.939230484541328,-1.15022560655515E-16,0.));
#16417=CARTESIAN_POINT('Origin',(0.,0.,0.));
#16418=CARTESIAN_POINT('',(0.839230484541328,-1.02776092664042E-16,-0.1));
#16419=CARTESIAN_POINT('Origin',(0.939230484541328,-1.15022560655515E-16,
-0.1));
#16420=CARTESIAN_POINT('Origin',(0.,0.,-0.1));
#16421=CARTESIAN_POINT('Origin',(-0.839230484541328,0.,-7.24797437703358E-18));
#16422=CARTESIAN_POINT('',(2.15,-2.63299061816681E-16,0.));
#16423=CARTESIAN_POINT('Origin',(0.,0.,0.));
#16424=CARTESIAN_POINT('Origin',(0.,0.,-0.0749999999999998));
#16425=CARTESIAN_POINT('',(0.839230484541328,-1.02776092664042E-16,-0.15));
#16426=CARTESIAN_POINT('Origin',(0.,0.,-0.15));
#16427=CARTESIAN_POINT('',(0.839230484541328,-1.02776092664042E-16,-0.0749999999999998));
#16428=CARTESIAN_POINT('Origin',(0.,0.,-0.45));
#16429=CARTESIAN_POINT('',(0.96675,-1.1839272930757E-16,-0.625909310648334));
#16430=CARTESIAN_POINT('Origin',(0.,0.,-0.625909310648334));
#16431=CARTESIAN_POINT('',(0.919615242270664,-1.12620386289389E-16,-0.45));
#16432=CARTESIAN_POINT('Origin',(0.,0.,-3.375));
#16433=CARTESIAN_POINT('',(0.96675,1.1839272930757E-16,-6.));
#16434=CARTESIAN_POINT('Origin',(0.,0.,-6.));
#16435=CARTESIAN_POINT('',(0.96675,-1.1839272930757E-16,-3.375));
#16436=CARTESIAN_POINT('Origin',(0.,0.,-6.));
#16437=CARTESIAN_POINT('Origin',(7.21644966006352E-15,0.,-5.12965591734105));
#16438=CARTESIAN_POINT('',(-2.07563463599418,0.,0.85));
#16439=CARTESIAN_POINT('Origin',(7.21644966006352E-15,0.,-5.12965591734105));
#16440=CARTESIAN_POINT('',(2.07563463599418,-2.54191931316966E-16,0.85));
#16441=CARTESIAN_POINT('Origin',(0.,0.,0.85));
#16442=CARTESIAN_POINT('Origin',(0.,0.,0.85));
#16443=CARTESIAN_POINT('Origin',(0.,0.,0.425));
#16444=CARTESIAN_POINT('',(2.11281731799709,-2.58745496566823E-16,0.425));
#16445=CARTESIAN_POINT('',(0.,0.,0.));
#16446=CARTESIAN_POINT('Origin',(-0.744000000195138,0.744000000196221,1.2));
#16447=CARTESIAN_POINT('',(-0.744000000195138,0.248000000196221,1.15122809938326));
#16448=CARTESIAN_POINT('',(-0.248000000195138,0.744000000196666,1.15122809938313));
#16449=CARTESIAN_POINT('Ctrl Pts',(-0.744000000195138,0.248000000196221,
1.15122809938326));
#16450=CARTESIAN_POINT('Ctrl Pts',(-0.743548129195526,0.248000000196221,
1.15128162561029));
#16451=CARTESIAN_POINT('Ctrl Pts',(-0.743096462399636,0.248000617700407,
1.15133505381795));
#16452=CARTESIAN_POINT('Ctrl Pts',(-0.68084251616827,0.248170686680912,
1.1586889909138));
#16453=CARTESIAN_POINT('Ctrl Pts',(-0.614748859330863,0.260619583354249,
1.16502989619583));
#16454=CARTESIAN_POINT('Ctrl Pts',(-0.492966510303847,0.311166686726808,
1.17344391775669));
#16455=CARTESIAN_POINT('Ctrl Pts',(-0.437280006866291,0.349270066587974,
1.17551763482271));
#16456=CARTESIAN_POINT('Ctrl Pts',(-0.393275036726453,0.393275036727851,
1.17551763482269));
#16457=CARTESIAN_POINT('Ctrl Pts',(-0.349270066586615,0.437280006867729,
1.17551763482268));
#16458=CARTESIAN_POINT('Ctrl Pts',(-0.3111666867255,0.49296651030532,1.17344391775664));
#16459=CARTESIAN_POINT('Ctrl Pts',(-0.26061958335305,0.61474885933238,1.16502989619573));
#16460=CARTESIAN_POINT('Ctrl Pts',(-0.248170686679772,0.680842516169798,
1.15868899091368));
#16461=CARTESIAN_POINT('Ctrl Pts',(-0.248000617699323,0.743096462401038,
1.15133505381783));
#16462=CARTESIAN_POINT('Ctrl Pts',(-0.248000000195138,0.743548129196929,
1.15128162561017));
#16463=CARTESIAN_POINT('Ctrl Pts',(-0.248000000195138,0.744000000196666,
1.15122809938313));
#16464=CARTESIAN_POINT('',(-0.744000000195138,0.248000000196221,0.583389912843141));
#16465=CARTESIAN_POINT('',(-0.744000000195138,0.248000000196221,1.2));
#16466=CARTESIAN_POINT('',(-0.516876228118667,0.303056928861888,0.19));
#16467=CARTESIAN_POINT('Origin',(-0.744000000195138,0.744000000196221,0.583389912843142));
#16468=CARTESIAN_POINT('',(-0.303056928861701,0.51687622811801,0.19));
#16469=CARTESIAN_POINT('Origin',(-0.744000000195138,0.744000000196221,0.19));
#16470=CARTESIAN_POINT('',(-0.248000000195138,0.744000000196666,0.583389912846777));
#16471=CARTESIAN_POINT('Origin',(-0.744000000195138,0.744000000196221,0.583389912847341));
#16472=CARTESIAN_POINT('',(-0.248000000195138,0.744000000196666,1.2));
#16473=CARTESIAN_POINT('Origin',(-0.248000000194694,0.24800000019315,1.2));
#16474=CARTESIAN_POINT('',(-0.24800000019541,1.04682989872245,1.10790668314437));
#16475=CARTESIAN_POINT('Origin',(-0.248000000194471,-2.22346593631069E-13,
-5.12965591734105));
#16476=CARTESIAN_POINT('',(-0.248000000195362,0.993500000023809,1.01553658903582));
#16477=CARTESIAN_POINT('Origin',(-0.248000000195457,1.09999999999962,1.2));
#16478=CARTESIAN_POINT('',(0.248000000196041,1.04682989872314,1.10790668314423));
#16479=CARTESIAN_POINT('Origin',(2.9811416492917E-12,-1.91582141081592,
-4.02355591008723));
#16480=CARTESIAN_POINT('',(0.303056928861511,0.516876228118951,0.19));
#16481=CARTESIAN_POINT('',(-0.124000000097707,0.516876228118288,0.19));
#16482=CARTESIAN_POINT('',(0.248000000196085,0.744000000194883,0.583389912842355));
#16483=CARTESIAN_POINT('Origin',(0.744000000196085,0.744000000194955,0.583389912841147));
#16484=CARTESIAN_POINT('',(0.248000000196033,1.1000000000003,1.19999999999985));
#16485=CARTESIAN_POINT('Origin',(0.248000000196033,1.10000000000039,1.2));
#16486=CARTESIAN_POINT('',(0.248000000196085,0.744000000194883,1.1512280993833));
#16487=CARTESIAN_POINT('Origin',(0.248000000196193,3.61135222251268E-14,
-5.12965591734105));
#16488=CARTESIAN_POINT('',(0.248000000196085,0.744000000194883,1.2));
#16489=CARTESIAN_POINT('Origin',(0.744000000196085,0.744000000194955,1.2));
#16490=CARTESIAN_POINT('',(0.744000000196732,0.248000000194955,1.15122809938313));
#16491=CARTESIAN_POINT('Ctrl Pts',(0.248000000196085,0.744000000194883,
1.1512280993833));
#16492=CARTESIAN_POINT('Ctrl Pts',(0.248000000196085,0.743548129195249,
1.15128162561033));
#16493=CARTESIAN_POINT('Ctrl Pts',(0.24800061770027,0.743096462399337,1.15133505381799));
#16494=CARTESIAN_POINT('Ctrl Pts',(0.248170686680793,0.68084251616795,1.15868899091384));
#16495=CARTESIAN_POINT('Ctrl Pts',(0.260619583354148,0.614748859330546,
1.16502989619587));
#16496=CARTESIAN_POINT('Ctrl Pts',(0.311166686726741,0.492966510303544,
1.17344391775672));
#16497=CARTESIAN_POINT('Ctrl Pts',(0.349270066587923,0.437280006865998,
1.17551763482273));
#16498=CARTESIAN_POINT('Ctrl Pts',(0.393275036727812,0.393275036726173,
1.17551763482271));
#16499=CARTESIAN_POINT('Ctrl Pts',(0.437280006867702,0.349270066586347,
1.1755176348227));
#16500=CARTESIAN_POINT('Ctrl Pts',(0.492966510305304,0.311166686725247,
1.17344391775665));
#16501=CARTESIAN_POINT('Ctrl Pts',(0.614748859332378,0.26061958335283,1.16502989619575));
#16502=CARTESIAN_POINT('Ctrl Pts',(0.6808425161698,0.248170686679572,1.15868899091369));
#16503=CARTESIAN_POINT('Ctrl Pts',(0.743096462401062,0.24800061769914,1.15133505381783));
#16504=CARTESIAN_POINT('Ctrl Pts',(0.743548129196974,0.248000000194955,
1.15128162561017));
#16505=CARTESIAN_POINT('Ctrl Pts',(0.744000000196732,0.248000000194955,
1.15122809938313));
#16506=CARTESIAN_POINT('',(0.516876228118432,0.30305692886123,0.19));
#16507=CARTESIAN_POINT('Origin',(0.744000000196085,0.744000000194955,0.19));
#16508=CARTESIAN_POINT('',(0.744000000196732,0.248000000194955,0.583389912846289));
#16509=CARTESIAN_POINT('Origin',(0.744000000196085,0.744000000194955,0.583389912845349));
#16510=CARTESIAN_POINT('',(0.744000000196732,0.248000000194955,1.2));
#16511=CARTESIAN_POINT('Origin',(0.248000000196157,0.248000000194308,1.2));
#16512=CARTESIAN_POINT('',(1.04682989872277,0.24800000019535,1.10790668314432));
#16513=CARTESIAN_POINT('Origin',(-3.16340915708764E-13,0.248000000193984,
-5.12965591734105));
#16514=CARTESIAN_POINT('',(0.99350000002449,0.248000000195281,1.01553658903639));
#16515=CARTESIAN_POINT('Origin',(1.09999999999997,0.248000000195419,1.2));
#16516=CARTESIAN_POINT('',(1.04682989872287,-0.248000000195507,1.1079066831443));
#16517=CARTESIAN_POINT('Origin',(-1.91582141081591,-4.04170800382928E-13,
-4.02355591008723));
#16518=CARTESIAN_POINT('',(0.51687622811856,-0.3030569288607,0.19));
#16519=CARTESIAN_POINT('',(0.51687622811847,0.124000000097702,0.19));
#16520=CARTESIAN_POINT('',(0.744000000195517,-0.248000000195115,0.583389912844004));
#16521=CARTESIAN_POINT('Origin',(0.744000000194874,-0.744000000195115,0.583389912842708));
#16522=CARTESIAN_POINT('',(1.09999999999998,-0.248000000195576,1.19999999999984));
#16523=CARTESIAN_POINT('Origin',(1.10000000000007,-0.248000000195576,1.2));
#16524=CARTESIAN_POINT('',(0.744000000195517,-0.248000000195115,1.15122809938326));
#16525=CARTESIAN_POINT('Origin',(-3.14351440352569E-13,-0.24800000019415,
-5.12965591734105));
#16526=CARTESIAN_POINT('',(0.744000000195517,-0.248000000195115,1.2));
#16527=CARTESIAN_POINT('Origin',(-0.744000000195415,-0.744000000194864,
1.2));
#16528=CARTESIAN_POINT('',(-0.248000000195415,-0.744000000196249,1.15122809938316));
#16529=CARTESIAN_POINT('',(-0.744000000196312,-0.248000000194864,1.15122809938318));
#16530=CARTESIAN_POINT('Ctrl Pts',(-0.248000000195415,-0.744000000196249,
1.15122809938316));
#16531=CARTESIAN_POINT('Ctrl Pts',(-0.248000000195414,-0.74354812919633,
1.15128162561023));
#16532=CARTESIAN_POINT('Ctrl Pts',(-0.248000617699598,-0.743096462400134,
1.15133505381792));
#16533=CARTESIAN_POINT('Ctrl Pts',(-0.248170686680046,-0.680842516168463,
1.15868899091381));
#16534=CARTESIAN_POINT('Ctrl Pts',(-0.260619583353321,-0.614748859331044,
1.16502989619585));
#16535=CARTESIAN_POINT('Ctrl Pts',(-0.311166686725766,-0.49296651030398,
1.17344391775673));
#16536=CARTESIAN_POINT('Ctrl Pts',(-0.349270066586879,-0.437280006866388,
1.17551763482276));
#16537=CARTESIAN_POINT('Ctrl Pts',(-0.393275036726715,-0.393275036726509,
1.17551763482276));
#16538=CARTESIAN_POINT('Ctrl Pts',(-0.437280006866551,-0.349270066586629,
1.17551763482276));
#16539=CARTESIAN_POINT('Ctrl Pts',(-0.492966510304106,-0.311166686725461,
1.17344391775673));
#16540=CARTESIAN_POINT('Ctrl Pts',(-0.61474885933112,-0.260619583352896,
1.16502989619586));
#16541=CARTESIAN_POINT('Ctrl Pts',(-0.680842516168527,-0.248170686679557,
1.15868899091382));
#16542=CARTESIAN_POINT('Ctrl Pts',(-0.743096462400073,-0.248000617699049,
1.15133505381795));
#16543=CARTESIAN_POINT('Ctrl Pts',(-0.74354812919627,-0.248000000194863,
1.15128162561025));
#16544=CARTESIAN_POINT('Ctrl Pts',(-0.744000000196312,-0.248000000194864,
1.15122809938318));
#16545=CARTESIAN_POINT('',(-0.248000000195415,-0.744000000196249,0.58338991284606));
#16546=CARTESIAN_POINT('',(-0.248000000195415,-0.744000000196249,1.2));
#16547=CARTESIAN_POINT('',(-0.303056928861281,-0.516876228118006,0.19));
#16548=CARTESIAN_POINT('Origin',(-0.744000000195415,-0.744000000194864,
0.583389912845007));
#16549=CARTESIAN_POINT('',(-0.516876228118667,-0.303056928860673,0.19));
#16550=CARTESIAN_POINT('Origin',(-0.744000000195415,-0.744000000194864,
0.19));
#16551=CARTESIAN_POINT('',(-0.744000000196312,-0.248000000194864,0.583389912845176));
#16552=CARTESIAN_POINT('Origin',(-0.744000000195415,-0.744000000194864,
0.583389912843621));
#16553=CARTESIAN_POINT('',(-0.744000000196312,-0.248000000194864,1.2));
#16554=CARTESIAN_POINT('Origin',(-0.24800000019403,-0.248000000193966,1.2));
#16555=CARTESIAN_POINT('',(-1.04682989872298,-0.248000000195412,1.10790668314428));
#16556=CARTESIAN_POINT('Origin',(4.5589868649524E-13,-0.248000000193518,
-5.12965591734105));
#16557=CARTESIAN_POINT('',(-0.993500000024419,-0.248000000195315,1.01553658903588));
#16558=CARTESIAN_POINT('Origin',(0.744000000194874,-0.744000000195115,1.2));
#16559=CARTESIAN_POINT('',(0.248000000194874,-0.744000000196067,1.15122809938321));
#16560=CARTESIAN_POINT('Ctrl Pts',(0.744000000195517,-0.248000000195115,
1.15122809938326));
#16561=CARTESIAN_POINT('Ctrl Pts',(0.743548129195714,-0.248000000195114,
1.15128162561031));
#16562=CARTESIAN_POINT('Ctrl Pts',(0.743096462399633,-0.248000617699299,
1.15133505381799));
#16563=CARTESIAN_POINT('Ctrl Pts',(0.680842516168076,-0.248170686679796,
1.15868899091386));
#16564=CARTESIAN_POINT('Ctrl Pts',(0.614748859330666,-0.260619583353124,
1.1650298961959));
#16565=CARTESIAN_POINT('Ctrl Pts',(0.492966510303643,-0.311166686725667,
1.17344391775676));
#16566=CARTESIAN_POINT('Ctrl Pts',(0.437280006866081,-0.349270066586825,
1.17551763482279));
#16567=CARTESIAN_POINT('Ctrl Pts',(0.393275036726237,-0.393275036726696,
1.17551763482278));
#16568=CARTESIAN_POINT('Ctrl Pts',(0.349270066586393,-0.437280006866568,
1.17551763482278));
#16569=CARTESIAN_POINT('Ctrl Pts',(0.31116668672527,-0.492966510304154,
1.17344391775674));
#16570=CARTESIAN_POINT('Ctrl Pts',(0.260619583352803,-0.614748859331208,
1.16502989619586));
#16571=CARTESIAN_POINT('Ctrl Pts',(0.248170686679517,-0.680842516168625,
1.15868899091381));
#16572=CARTESIAN_POINT('Ctrl Pts',(0.248000617699059,-0.743096462400057,
1.15133505381795));
#16573=CARTESIAN_POINT('Ctrl Pts',(0.248000000194873,-0.743548129196139,
1.15128162561027));
#16574=CARTESIAN_POINT('Ctrl Pts',(0.248000000194874,-0.744000000196067,
1.15122809938321));
#16575=CARTESIAN_POINT('',(0.30305692886038,-0.516876228118955,0.19));
#16576=CARTESIAN_POINT('Origin',(0.744000000194874,-0.744000000195115,0.19));
#16577=CARTESIAN_POINT('',(0.248000000194874,-0.744000000196067,0.5833899128444));
#16578=CARTESIAN_POINT('Origin',(0.744000000194874,-0.744000000195115,0.583389912841405));
#16579=CARTESIAN_POINT('',(0.248000000194874,-0.744000000196067,1.2));
#16580=CARTESIAN_POINT('Origin',(0.248000000193922,-0.248000000194471,1.2));
#16581=CARTESIAN_POINT('',(0.248000000195456,-1.04682989872316,1.10790668314425));
#16582=CARTESIAN_POINT('Origin',(0.248000000193446,4.75999652275667E-13,
-5.12965591734105));
#16583=CARTESIAN_POINT('',(0.248000000195353,-0.993500000024651,1.01553658903593));
#16584=CARTESIAN_POINT('Origin',(-1.10000000000019,0.248000000196221,1.2));
#16585=CARTESIAN_POINT('',(-1.04682989872296,0.248000000196221,1.10790668314426));
#16586=CARTESIAN_POINT('Origin',(7.17605422133295E-15,0.248000000196221,
-5.12965591734105));
#16587=CARTESIAN_POINT('',(-1.10000000000019,0.248000000196221,1.2));
#16588=CARTESIAN_POINT('Origin',(-1.10000000000019,-0.248000000195508,1.2));
#16589=CARTESIAN_POINT('',(-1.04942373620595,-1.28517341949389E-16,1.11239934145138));
#16590=CARTESIAN_POINT('Origin',(1.91582141081578,-5.36035544273609E-16,
-4.02355591008731));
#16591=CARTESIAN_POINT('',(-0.516876228118667,-0.124000000097755,0.19));
#16592=CARTESIAN_POINT('Origin',(1.91582141081578,-5.36035544273609E-16,
-4.02355591008731));
#16593=CARTESIAN_POINT('Origin',(-0.248000000196409,-1.09999999999961,1.2));
#16594=CARTESIAN_POINT('',(-0.24800000019626,-1.04682989872243,1.10790668314434));
#16595=CARTESIAN_POINT('Origin',(-0.248000000193338,6.92337424395539E-13,
-5.12965591734105));
#16596=CARTESIAN_POINT('',(-0.248000000196409,-1.09999999999954,1.19999999999987));
#16597=CARTESIAN_POINT('Origin',(0.248000000195558,-1.10000000000039,1.2));
#16598=CARTESIAN_POINT('Origin',(3.00794342650252E-12,1.91582141081592,
-4.02355591008723));
#16599=CARTESIAN_POINT('',(0.124000000097801,-0.516876228118675,0.19));
#16600=CARTESIAN_POINT('Origin',(-5.91193760612896E-14,-1.66533453693773E-15,
0.19));
#16601=CARTESIAN_POINT('Origin',(0.,0.,-0.1));
#16602=CARTESIAN_POINT('',(0.939230484541328,-1.15022560655515E-16,0.));
#16603=CARTESIAN_POINT('Origin',(0.,0.,0.));
#16604=CARTESIAN_POINT('',(0.839230484541328,-1.02776092664042E-16,-0.1));
#16605=CARTESIAN_POINT('Origin',(0.939230484541328,-1.15022560655515E-16,
-0.1));
#16606=CARTESIAN_POINT('Origin',(0.,0.,-0.1));
#16607=CARTESIAN_POINT('Origin',(-0.839230484541328,0.,-7.24797437703358E-18));
#16608=CARTESIAN_POINT('',(2.15,-2.63299061816681E-16,0.));
#16609=CARTESIAN_POINT('Origin',(0.,0.,0.));
#16610=CARTESIAN_POINT('Origin',(0.,0.,-0.0749999999999998));
#16611=CARTESIAN_POINT('',(0.839230484541328,-1.02776092664042E-16,-0.15));
#16612=CARTESIAN_POINT('Origin',(0.,0.,-0.15));
#16613=CARTESIAN_POINT('',(0.839230484541328,-1.02776092664042E-16,-0.0749999999999998));
#16614=CARTESIAN_POINT('Origin',(0.,0.,-0.45));
#16615=CARTESIAN_POINT('',(0.96675,-1.1839272930757E-16,-0.625909310648334));
#16616=CARTESIAN_POINT('Origin',(0.,0.,-0.625909310648334));
#16617=CARTESIAN_POINT('',(0.919615242270664,-1.12620386289389E-16,-0.45));
#16618=CARTESIAN_POINT('Origin',(0.,0.,-3.375));
#16619=CARTESIAN_POINT('',(0.96675,1.1839272930757E-16,-6.));
#16620=CARTESIAN_POINT('Origin',(0.,0.,-6.));
#16621=CARTESIAN_POINT('',(0.96675,-1.1839272930757E-16,-3.375));
#16622=CARTESIAN_POINT('Origin',(0.,0.,-6.));
#16623=CARTESIAN_POINT('Origin',(7.21644966006352E-15,0.,-5.12965591734105));
#16624=CARTESIAN_POINT('',(-2.07563463599418,0.,0.85));
#16625=CARTESIAN_POINT('Origin',(7.21644966006352E-15,0.,-5.12965591734105));
#16626=CARTESIAN_POINT('',(2.07563463599418,-2.54191931316966E-16,0.85));
#16627=CARTESIAN_POINT('Origin',(0.,0.,0.85));
#16628=CARTESIAN_POINT('Origin',(0.,0.,0.85));
#16629=CARTESIAN_POINT('Origin',(0.,0.,0.425));
#16630=CARTESIAN_POINT('',(2.11281731799709,-2.58745496566823E-16,0.425));
#16631=CARTESIAN_POINT('',(0.,0.,0.));
#16632=CARTESIAN_POINT('Origin',(-0.744000000195138,0.744000000196221,1.2));
#16633=CARTESIAN_POINT('',(-0.744000000195138,0.248000000196221,1.15122809938326));
#16634=CARTESIAN_POINT('',(-0.248000000195138,0.744000000196666,1.15122809938313));
#16635=CARTESIAN_POINT('Ctrl Pts',(-0.744000000195138,0.248000000196221,
1.15122809938326));
#16636=CARTESIAN_POINT('Ctrl Pts',(-0.743548129195526,0.248000000196221,
1.15128162561029));
#16637=CARTESIAN_POINT('Ctrl Pts',(-0.743096462399636,0.248000617700407,
1.15133505381795));
#16638=CARTESIAN_POINT('Ctrl Pts',(-0.68084251616827,0.248170686680912,
1.1586889909138));
#16639=CARTESIAN_POINT('Ctrl Pts',(-0.614748859330863,0.260619583354249,
1.16502989619583));
#16640=CARTESIAN_POINT('Ctrl Pts',(-0.492966510303847,0.311166686726808,
1.17344391775669));
#16641=CARTESIAN_POINT('Ctrl Pts',(-0.437280006866291,0.349270066587974,
1.17551763482271));
#16642=CARTESIAN_POINT('Ctrl Pts',(-0.393275036726453,0.393275036727851,
1.17551763482269));
#16643=CARTESIAN_POINT('Ctrl Pts',(-0.349270066586615,0.437280006867729,
1.17551763482268));
#16644=CARTESIAN_POINT('Ctrl Pts',(-0.3111666867255,0.49296651030532,1.17344391775664));
#16645=CARTESIAN_POINT('Ctrl Pts',(-0.26061958335305,0.61474885933238,1.16502989619573));
#16646=CARTESIAN_POINT('Ctrl Pts',(-0.248170686679772,0.680842516169798,
1.15868899091368));
#16647=CARTESIAN_POINT('Ctrl Pts',(-0.248000617699323,0.743096462401038,
1.15133505381783));
#16648=CARTESIAN_POINT('Ctrl Pts',(-0.248000000195138,0.743548129196929,
1.15128162561017));
#16649=CARTESIAN_POINT('Ctrl Pts',(-0.248000000195138,0.744000000196666,
1.15122809938313));
#16650=CARTESIAN_POINT('',(-0.744000000195138,0.248000000196221,0.583389912843141));
#16651=CARTESIAN_POINT('',(-0.744000000195138,0.248000000196221,1.2));
#16652=CARTESIAN_POINT('',(-0.516876228118667,0.303056928861888,0.19));
#16653=CARTESIAN_POINT('Origin',(-0.744000000195138,0.744000000196221,0.583389912843142));
#16654=CARTESIAN_POINT('',(-0.303056928861701,0.51687622811801,0.19));
#16655=CARTESIAN_POINT('Origin',(-0.744000000195138,0.744000000196221,0.19));
#16656=CARTESIAN_POINT('',(-0.248000000195138,0.744000000196666,0.583389912846777));
#16657=CARTESIAN_POINT('Origin',(-0.744000000195138,0.744000000196221,0.583389912847341));
#16658=CARTESIAN_POINT('',(-0.248000000195138,0.744000000196666,1.2));
#16659=CARTESIAN_POINT('Origin',(-0.248000000194694,0.24800000019315,1.2));
#16660=CARTESIAN_POINT('',(-0.24800000019541,1.04682989872245,1.10790668314437));
#16661=CARTESIAN_POINT('Origin',(-0.248000000194471,-2.22346593631069E-13,
-5.12965591734105));
#16662=CARTESIAN_POINT('',(-0.248000000195362,0.993500000023809,1.01553658903582));
#16663=CARTESIAN_POINT('Origin',(-0.248000000195457,1.09999999999962,1.2));
#16664=CARTESIAN_POINT('',(0.248000000196041,1.04682989872314,1.10790668314423));
#16665=CARTESIAN_POINT('Origin',(2.9811416492917E-12,-1.91582141081592,
-4.02355591008723));
#16666=CARTESIAN_POINT('',(0.303056928861511,0.516876228118951,0.19));
#16667=CARTESIAN_POINT('',(-0.124000000097707,0.516876228118288,0.19));
#16668=CARTESIAN_POINT('',(0.248000000196085,0.744000000194883,0.583389912842355));
#16669=CARTESIAN_POINT('Origin',(0.744000000196085,0.744000000194955,0.583389912841147));
#16670=CARTESIAN_POINT('',(0.248000000196033,1.1000000000003,1.19999999999985));
#16671=CARTESIAN_POINT('Origin',(0.248000000196033,1.10000000000039,1.2));
#16672=CARTESIAN_POINT('',(0.248000000196085,0.744000000194883,1.1512280993833));
#16673=CARTESIAN_POINT('Origin',(0.248000000196193,3.61135222251268E-14,
-5.12965591734105));
#16674=CARTESIAN_POINT('',(0.248000000196085,0.744000000194883,1.2));
#16675=CARTESIAN_POINT('Origin',(0.744000000196085,0.744000000194955,1.2));
#16676=CARTESIAN_POINT('',(0.744000000196732,0.248000000194955,1.15122809938313));
#16677=CARTESIAN_POINT('Ctrl Pts',(0.248000000196085,0.744000000194883,
1.1512280993833));
#16678=CARTESIAN_POINT('Ctrl Pts',(0.248000000196085,0.743548129195249,
1.15128162561033));
#16679=CARTESIAN_POINT('Ctrl Pts',(0.24800061770027,0.743096462399337,1.15133505381799));
#16680=CARTESIAN_POINT('Ctrl Pts',(0.248170686680793,0.68084251616795,1.15868899091384));
#16681=CARTESIAN_POINT('Ctrl Pts',(0.260619583354148,0.614748859330546,
1.16502989619587));
#16682=CARTESIAN_POINT('Ctrl Pts',(0.311166686726741,0.492966510303544,
1.17344391775672));
#16683=CARTESIAN_POINT('Ctrl Pts',(0.349270066587923,0.437280006865998,
1.17551763482273));
#16684=CARTESIAN_POINT('Ctrl Pts',(0.393275036727812,0.393275036726173,
1.17551763482271));
#16685=CARTESIAN_POINT('Ctrl Pts',(0.437280006867702,0.349270066586347,
1.1755176348227));
#16686=CARTESIAN_POINT('Ctrl Pts',(0.492966510305304,0.311166686725247,
1.17344391775665));
#16687=CARTESIAN_POINT('Ctrl Pts',(0.614748859332378,0.26061958335283,1.16502989619575));
#16688=CARTESIAN_POINT('Ctrl Pts',(0.6808425161698,0.248170686679572,1.15868899091369));
#16689=CARTESIAN_POINT('Ctrl Pts',(0.743096462401062,0.24800061769914,1.15133505381783));
#16690=CARTESIAN_POINT('Ctrl Pts',(0.743548129196974,0.248000000194955,
1.15128162561017));
#16691=CARTESIAN_POINT('Ctrl Pts',(0.744000000196732,0.248000000194955,
1.15122809938313));
#16692=CARTESIAN_POINT('',(0.516876228118432,0.30305692886123,0.19));
#16693=CARTESIAN_POINT('Origin',(0.744000000196085,0.744000000194955,0.19));
#16694=CARTESIAN_POINT('',(0.744000000196732,0.248000000194955,0.583389912846289));
#16695=CARTESIAN_POINT('Origin',(0.744000000196085,0.744000000194955,0.583389912845349));
#16696=CARTESIAN_POINT('',(0.744000000196732,0.248000000194955,1.2));
#16697=CARTESIAN_POINT('Origin',(0.248000000196157,0.248000000194308,1.2));
#16698=CARTESIAN_POINT('',(1.04682989872277,0.24800000019535,1.10790668314432));
#16699=CARTESIAN_POINT('Origin',(-3.16340915708764E-13,0.248000000193984,
-5.12965591734105));
#16700=CARTESIAN_POINT('',(0.99350000002449,0.248000000195281,1.01553658903639));
#16701=CARTESIAN_POINT('Origin',(1.09999999999997,0.248000000195419,1.2));
#16702=CARTESIAN_POINT('',(1.04682989872287,-0.248000000195507,1.1079066831443));
#16703=CARTESIAN_POINT('Origin',(-1.91582141081591,-4.04170800382928E-13,
-4.02355591008723));
#16704=CARTESIAN_POINT('',(0.51687622811856,-0.3030569288607,0.19));
#16705=CARTESIAN_POINT('',(0.51687622811847,0.124000000097702,0.19));
#16706=CARTESIAN_POINT('',(0.744000000195517,-0.248000000195115,0.583389912844004));
#16707=CARTESIAN_POINT('Origin',(0.744000000194874,-0.744000000195115,0.583389912842708));
#16708=CARTESIAN_POINT('',(1.09999999999998,-0.248000000195576,1.19999999999984));
#16709=CARTESIAN_POINT('Origin',(1.10000000000007,-0.248000000195576,1.2));
#16710=CARTESIAN_POINT('',(0.744000000195517,-0.248000000195115,1.15122809938326));
#16711=CARTESIAN_POINT('Origin',(-3.14351440352569E-13,-0.24800000019415,
-5.12965591734105));
#16712=CARTESIAN_POINT('',(0.744000000195517,-0.248000000195115,1.2));
#16713=CARTESIAN_POINT('Origin',(-0.744000000195415,-0.744000000194864,
1.2));
#16714=CARTESIAN_POINT('',(-0.248000000195415,-0.744000000196249,1.15122809938316));
#16715=CARTESIAN_POINT('',(-0.744000000196312,-0.248000000194864,1.15122809938318));
#16716=CARTESIAN_POINT('Ctrl Pts',(-0.248000000195415,-0.744000000196249,
1.15122809938316));
#16717=CARTESIAN_POINT('Ctrl Pts',(-0.248000000195414,-0.74354812919633,
1.15128162561023));
#16718=CARTESIAN_POINT('Ctrl Pts',(-0.248000617699598,-0.743096462400134,
1.15133505381792));
#16719=CARTESIAN_POINT('Ctrl Pts',(-0.248170686680046,-0.680842516168463,
1.15868899091381));
#16720=CARTESIAN_POINT('Ctrl Pts',(-0.260619583353321,-0.614748859331044,
1.16502989619585));
#16721=CARTESIAN_POINT('Ctrl Pts',(-0.311166686725766,-0.49296651030398,
1.17344391775673));
#16722=CARTESIAN_POINT('Ctrl Pts',(-0.349270066586879,-0.437280006866388,
1.17551763482276));
#16723=CARTESIAN_POINT('Ctrl Pts',(-0.393275036726715,-0.393275036726509,
1.17551763482276));
#16724=CARTESIAN_POINT('Ctrl Pts',(-0.437280006866551,-0.349270066586629,
1.17551763482276));
#16725=CARTESIAN_POINT('Ctrl Pts',(-0.492966510304106,-0.311166686725461,
1.17344391775673));
#16726=CARTESIAN_POINT('Ctrl Pts',(-0.61474885933112,-0.260619583352896,
1.16502989619586));
#16727=CARTESIAN_POINT('Ctrl Pts',(-0.680842516168527,-0.248170686679557,
1.15868899091382));
#16728=CARTESIAN_POINT('Ctrl Pts',(-0.743096462400073,-0.248000617699049,
1.15133505381795));
#16729=CARTESIAN_POINT('Ctrl Pts',(-0.74354812919627,-0.248000000194863,
1.15128162561025));
#16730=CARTESIAN_POINT('Ctrl Pts',(-0.744000000196312,-0.248000000194864,
1.15122809938318));
#16731=CARTESIAN_POINT('',(-0.248000000195415,-0.744000000196249,0.58338991284606));
#16732=CARTESIAN_POINT('',(-0.248000000195415,-0.744000000196249,1.2));
#16733=CARTESIAN_POINT('',(-0.303056928861281,-0.516876228118006,0.19));
#16734=CARTESIAN_POINT('Origin',(-0.744000000195415,-0.744000000194864,
0.583389912845007));
#16735=CARTESIAN_POINT('',(-0.516876228118667,-0.303056928860673,0.19));
#16736=CARTESIAN_POINT('Origin',(-0.744000000195415,-0.744000000194864,
0.19));
#16737=CARTESIAN_POINT('',(-0.744000000196312,-0.248000000194864,0.583389912845176));
#16738=CARTESIAN_POINT('Origin',(-0.744000000195415,-0.744000000194864,
0.583389912843621));
#16739=CARTESIAN_POINT('',(-0.744000000196312,-0.248000000194864,1.2));
#16740=CARTESIAN_POINT('Origin',(-0.24800000019403,-0.248000000193966,1.2));
#16741=CARTESIAN_POINT('',(-1.04682989872298,-0.248000000195412,1.10790668314428));
#16742=CARTESIAN_POINT('Origin',(4.5589868649524E-13,-0.248000000193518,
-5.12965591734105));
#16743=CARTESIAN_POINT('',(-0.993500000024419,-0.248000000195315,1.01553658903588));
#16744=CARTESIAN_POINT('Origin',(0.744000000194874,-0.744000000195115,1.2));
#16745=CARTESIAN_POINT('',(0.248000000194874,-0.744000000196067,1.15122809938321));
#16746=CARTESIAN_POINT('Ctrl Pts',(0.744000000195517,-0.248000000195115,
1.15122809938326));
#16747=CARTESIAN_POINT('Ctrl Pts',(0.743548129195714,-0.248000000195114,
1.15128162561031));
#16748=CARTESIAN_POINT('Ctrl Pts',(0.743096462399633,-0.248000617699299,
1.15133505381799));
#16749=CARTESIAN_POINT('Ctrl Pts',(0.680842516168076,-0.248170686679796,
1.15868899091386));
#16750=CARTESIAN_POINT('Ctrl Pts',(0.614748859330666,-0.260619583353124,
1.1650298961959));
#16751=CARTESIAN_POINT('Ctrl Pts',(0.492966510303643,-0.311166686725667,
1.17344391775676));
#16752=CARTESIAN_POINT('Ctrl Pts',(0.437280006866081,-0.349270066586825,
1.17551763482279));
#16753=CARTESIAN_POINT('Ctrl Pts',(0.393275036726237,-0.393275036726696,
1.17551763482278));
#16754=CARTESIAN_POINT('Ctrl Pts',(0.349270066586393,-0.437280006866568,
1.17551763482278));
#16755=CARTESIAN_POINT('Ctrl Pts',(0.31116668672527,-0.492966510304154,
1.17344391775674));
#16756=CARTESIAN_POINT('Ctrl Pts',(0.260619583352803,-0.614748859331208,
1.16502989619586));
#16757=CARTESIAN_POINT('Ctrl Pts',(0.248170686679517,-0.680842516168625,
1.15868899091381));
#16758=CARTESIAN_POINT('Ctrl Pts',(0.248000617699059,-0.743096462400057,
1.15133505381795));
#16759=CARTESIAN_POINT('Ctrl Pts',(0.248000000194873,-0.743548129196139,
1.15128162561027));
#16760=CARTESIAN_POINT('Ctrl Pts',(0.248000000194874,-0.744000000196067,
1.15122809938321));
#16761=CARTESIAN_POINT('',(0.30305692886038,-0.516876228118955,0.19));
#16762=CARTESIAN_POINT('Origin',(0.744000000194874,-0.744000000195115,0.19));
#16763=CARTESIAN_POINT('',(0.248000000194874,-0.744000000196067,0.5833899128444));
#16764=CARTESIAN_POINT('Origin',(0.744000000194874,-0.744000000195115,0.583389912841405));
#16765=CARTESIAN_POINT('',(0.248000000194874,-0.744000000196067,1.2));
#16766=CARTESIAN_POINT('Origin',(0.248000000193922,-0.248000000194471,1.2));
#16767=CARTESIAN_POINT('',(0.248000000195456,-1.04682989872316,1.10790668314425));
#16768=CARTESIAN_POINT('Origin',(0.248000000193446,4.75999652275667E-13,
-5.12965591734105));
#16769=CARTESIAN_POINT('',(0.248000000195353,-0.993500000024651,1.01553658903593));
#16770=CARTESIAN_POINT('Origin',(-1.10000000000019,0.248000000196221,1.2));
#16771=CARTESIAN_POINT('',(-1.04682989872296,0.248000000196221,1.10790668314426));
#16772=CARTESIAN_POINT('Origin',(7.17605422133295E-15,0.248000000196221,
-5.12965591734105));
#16773=CARTESIAN_POINT('',(-1.10000000000019,0.248000000196221,1.2));
#16774=CARTESIAN_POINT('Origin',(-1.10000000000019,-0.248000000195508,1.2));
#16775=CARTESIAN_POINT('',(-1.04942373620595,-1.28517341949389E-16,1.11239934145138));
#16776=CARTESIAN_POINT('Origin',(1.91582141081578,-5.36035544273609E-16,
-4.02355591008731));
#16777=CARTESIAN_POINT('',(-0.516876228118667,-0.124000000097755,0.19));
#16778=CARTESIAN_POINT('Origin',(1.91582141081578,-5.36035544273609E-16,
-4.02355591008731));
#16779=CARTESIAN_POINT('Origin',(-0.248000000196409,-1.09999999999961,1.2));
#16780=CARTESIAN_POINT('',(-0.24800000019626,-1.04682989872243,1.10790668314434));
#16781=CARTESIAN_POINT('Origin',(-0.248000000193338,6.92337424395539E-13,
-5.12965591734105));
#16782=CARTESIAN_POINT('',(-0.248000000196409,-1.09999999999954,1.19999999999987));
#16783=CARTESIAN_POINT('Origin',(0.248000000195558,-1.10000000000039,1.2));
#16784=CARTESIAN_POINT('Origin',(3.00794342650252E-12,1.91582141081592,
-4.02355591008723));
#16785=CARTESIAN_POINT('',(0.124000000097801,-0.516876228118675,0.19));
#16786=CARTESIAN_POINT('Origin',(-5.91193760612896E-14,-1.66533453693773E-15,
0.19));
#16787=CARTESIAN_POINT('Origin',(0.,0.,-0.1));
#16788=CARTESIAN_POINT('',(0.939230484541328,-1.15022560655515E-16,0.));
#16789=CARTESIAN_POINT('Origin',(0.,0.,0.));
#16790=CARTESIAN_POINT('',(0.839230484541328,-1.02776092664042E-16,-0.1));
#16791=CARTESIAN_POINT('Origin',(0.939230484541328,-1.15022560655515E-16,
-0.1));
#16792=CARTESIAN_POINT('Origin',(0.,0.,-0.1));
#16793=CARTESIAN_POINT('Origin',(-0.839230484541328,0.,-7.24797437703358E-18));
#16794=CARTESIAN_POINT('',(2.15,-2.63299061816681E-16,0.));
#16795=CARTESIAN_POINT('Origin',(0.,0.,0.));
#16796=CARTESIAN_POINT('Origin',(0.,0.,-0.0749999999999998));
#16797=CARTESIAN_POINT('',(0.839230484541328,-1.02776092664042E-16,-0.15));
#16798=CARTESIAN_POINT('Origin',(0.,0.,-0.15));
#16799=CARTESIAN_POINT('',(0.839230484541328,-1.02776092664042E-16,-0.0749999999999998));
#16800=CARTESIAN_POINT('Origin',(0.,0.,-0.45));
#16801=CARTESIAN_POINT('',(0.96675,-1.1839272930757E-16,-0.625909310648334));
#16802=CARTESIAN_POINT('Origin',(0.,0.,-0.625909310648334));
#16803=CARTESIAN_POINT('',(0.919615242270664,-1.12620386289389E-16,-0.45));
#16804=CARTESIAN_POINT('Origin',(0.,0.,-3.375));
#16805=CARTESIAN_POINT('',(0.96675,1.1839272930757E-16,-6.));
#16806=CARTESIAN_POINT('Origin',(0.,0.,-6.));
#16807=CARTESIAN_POINT('',(0.96675,-1.1839272930757E-16,-3.375));
#16808=CARTESIAN_POINT('Origin',(0.,0.,-6.));
#16809=CARTESIAN_POINT('Origin',(7.21644966006352E-15,0.,-5.12965591734105));
#16810=CARTESIAN_POINT('',(-2.07563463599418,0.,0.85));
#16811=CARTESIAN_POINT('Origin',(7.21644966006352E-15,0.,-5.12965591734105));
#16812=CARTESIAN_POINT('',(2.07563463599418,-2.54191931316966E-16,0.85));
#16813=CARTESIAN_POINT('Origin',(0.,0.,0.85));
#16814=CARTESIAN_POINT('Origin',(0.,0.,0.85));
#16815=CARTESIAN_POINT('Origin',(0.,0.,0.425));
#16816=CARTESIAN_POINT('',(2.11281731799709,-2.58745496566823E-16,0.425));
#16817=CARTESIAN_POINT('',(0.,0.,0.));
#16818=CARTESIAN_POINT('Origin',(-0.744000000195138,0.744000000196221,1.2));
#16819=CARTESIAN_POINT('',(-0.744000000195138,0.248000000196221,1.15122809938326));
#16820=CARTESIAN_POINT('',(-0.248000000195138,0.744000000196666,1.15122809938313));
#16821=CARTESIAN_POINT('Ctrl Pts',(-0.744000000195138,0.248000000196221,
1.15122809938326));
#16822=CARTESIAN_POINT('Ctrl Pts',(-0.743548129195526,0.248000000196221,
1.15128162561029));
#16823=CARTESIAN_POINT('Ctrl Pts',(-0.743096462399636,0.248000617700407,
1.15133505381795));
#16824=CARTESIAN_POINT('Ctrl Pts',(-0.68084251616827,0.248170686680912,
1.1586889909138));
#16825=CARTESIAN_POINT('Ctrl Pts',(-0.614748859330863,0.260619583354249,
1.16502989619583));
#16826=CARTESIAN_POINT('Ctrl Pts',(-0.492966510303847,0.311166686726808,
1.17344391775669));
#16827=CARTESIAN_POINT('Ctrl Pts',(-0.437280006866291,0.349270066587974,
1.17551763482271));
#16828=CARTESIAN_POINT('Ctrl Pts',(-0.393275036726453,0.393275036727851,
1.17551763482269));
#16829=CARTESIAN_POINT('Ctrl Pts',(-0.349270066586615,0.437280006867729,
1.17551763482268));
#16830=CARTESIAN_POINT('Ctrl Pts',(-0.3111666867255,0.49296651030532,1.17344391775664));
#16831=CARTESIAN_POINT('Ctrl Pts',(-0.26061958335305,0.61474885933238,1.16502989619573));
#16832=CARTESIAN_POINT('Ctrl Pts',(-0.248170686679772,0.680842516169798,
1.15868899091368));
#16833=CARTESIAN_POINT('Ctrl Pts',(-0.248000617699323,0.743096462401038,
1.15133505381783));
#16834=CARTESIAN_POINT('Ctrl Pts',(-0.248000000195138,0.743548129196929,
1.15128162561017));
#16835=CARTESIAN_POINT('Ctrl Pts',(-0.248000000195138,0.744000000196666,
1.15122809938313));
#16836=CARTESIAN_POINT('',(-0.744000000195138,0.248000000196221,0.583389912843141));
#16837=CARTESIAN_POINT('',(-0.744000000195138,0.248000000196221,1.2));
#16838=CARTESIAN_POINT('',(-0.516876228118667,0.303056928861888,0.19));
#16839=CARTESIAN_POINT('Origin',(-0.744000000195138,0.744000000196221,0.583389912843142));
#16840=CARTESIAN_POINT('',(-0.303056928861701,0.51687622811801,0.19));
#16841=CARTESIAN_POINT('Origin',(-0.744000000195138,0.744000000196221,0.19));
#16842=CARTESIAN_POINT('',(-0.248000000195138,0.744000000196666,0.583389912846777));
#16843=CARTESIAN_POINT('Origin',(-0.744000000195138,0.744000000196221,0.583389912847341));
#16844=CARTESIAN_POINT('',(-0.248000000195138,0.744000000196666,1.2));
#16845=CARTESIAN_POINT('Origin',(-0.248000000194694,0.24800000019315,1.2));
#16846=CARTESIAN_POINT('',(-0.24800000019541,1.04682989872245,1.10790668314437));
#16847=CARTESIAN_POINT('Origin',(-0.248000000194471,-2.22346593631069E-13,
-5.12965591734105));
#16848=CARTESIAN_POINT('',(-0.248000000195362,0.993500000023809,1.01553658903582));
#16849=CARTESIAN_POINT('Origin',(-0.248000000195457,1.09999999999962,1.2));
#16850=CARTESIAN_POINT('',(0.248000000196041,1.04682989872314,1.10790668314423));
#16851=CARTESIAN_POINT('Origin',(2.9811416492917E-12,-1.91582141081592,
-4.02355591008723));
#16852=CARTESIAN_POINT('',(0.303056928861511,0.516876228118951,0.19));
#16853=CARTESIAN_POINT('',(-0.124000000097707,0.516876228118288,0.19));
#16854=CARTESIAN_POINT('',(0.248000000196085,0.744000000194883,0.583389912842355));
#16855=CARTESIAN_POINT('Origin',(0.744000000196085,0.744000000194955,0.583389912841147));
#16856=CARTESIAN_POINT('',(0.248000000196033,1.1000000000003,1.19999999999985));
#16857=CARTESIAN_POINT('Origin',(0.248000000196033,1.10000000000039,1.2));
#16858=CARTESIAN_POINT('',(0.248000000196085,0.744000000194883,1.1512280993833));
#16859=CARTESIAN_POINT('Origin',(0.248000000196193,3.61135222251268E-14,
-5.12965591734105));
#16860=CARTESIAN_POINT('',(0.248000000196085,0.744000000194883,1.2));
#16861=CARTESIAN_POINT('Origin',(0.744000000196085,0.744000000194955,1.2));
#16862=CARTESIAN_POINT('',(0.744000000196732,0.248000000194955,1.15122809938313));
#16863=CARTESIAN_POINT('Ctrl Pts',(0.248000000196085,0.744000000194883,
1.1512280993833));
#16864=CARTESIAN_POINT('Ctrl Pts',(0.248000000196085,0.743548129195249,
1.15128162561033));
#16865=CARTESIAN_POINT('Ctrl Pts',(0.24800061770027,0.743096462399337,1.15133505381799));
#16866=CARTESIAN_POINT('Ctrl Pts',(0.248170686680793,0.68084251616795,1.15868899091384));
#16867=CARTESIAN_POINT('Ctrl Pts',(0.260619583354148,0.614748859330546,
1.16502989619587));
#16868=CARTESIAN_POINT('Ctrl Pts',(0.311166686726741,0.492966510303544,
1.17344391775672));
#16869=CARTESIAN_POINT('Ctrl Pts',(0.349270066587923,0.437280006865998,
1.17551763482273));
#16870=CARTESIAN_POINT('Ctrl Pts',(0.393275036727812,0.393275036726173,
1.17551763482271));
#16871=CARTESIAN_POINT('Ctrl Pts',(0.437280006867702,0.349270066586347,
1.1755176348227));
#16872=CARTESIAN_POINT('Ctrl Pts',(0.492966510305304,0.311166686725247,
1.17344391775665));
#16873=CARTESIAN_POINT('Ctrl Pts',(0.614748859332378,0.26061958335283,1.16502989619575));
#16874=CARTESIAN_POINT('Ctrl Pts',(0.6808425161698,0.248170686679572,1.15868899091369));
#16875=CARTESIAN_POINT('Ctrl Pts',(0.743096462401062,0.24800061769914,1.15133505381783));
#16876=CARTESIAN_POINT('Ctrl Pts',(0.743548129196974,0.248000000194955,
1.15128162561017));
#16877=CARTESIAN_POINT('Ctrl Pts',(0.744000000196732,0.248000000194955,
1.15122809938313));
#16878=CARTESIAN_POINT('',(0.516876228118432,0.30305692886123,0.19));
#16879=CARTESIAN_POINT('Origin',(0.744000000196085,0.744000000194955,0.19));
#16880=CARTESIAN_POINT('',(0.744000000196732,0.248000000194955,0.583389912846289));
#16881=CARTESIAN_POINT('Origin',(0.744000000196085,0.744000000194955,0.583389912845349));
#16882=CARTESIAN_POINT('',(0.744000000196732,0.248000000194955,1.2));
#16883=CARTESIAN_POINT('Origin',(0.248000000196157,0.248000000194308,1.2));
#16884=CARTESIAN_POINT('',(1.04682989872277,0.24800000019535,1.10790668314432));
#16885=CARTESIAN_POINT('Origin',(-3.16340915708764E-13,0.248000000193984,
-5.12965591734105));
#16886=CARTESIAN_POINT('',(0.99350000002449,0.248000000195281,1.01553658903639));
#16887=CARTESIAN_POINT('Origin',(1.09999999999997,0.248000000195419,1.2));
#16888=CARTESIAN_POINT('',(1.04682989872287,-0.248000000195507,1.1079066831443));
#16889=CARTESIAN_POINT('Origin',(-1.91582141081591,-4.04170800382928E-13,
-4.02355591008723));
#16890=CARTESIAN_POINT('',(0.51687622811856,-0.3030569288607,0.19));
#16891=CARTESIAN_POINT('',(0.51687622811847,0.124000000097702,0.19));
#16892=CARTESIAN_POINT('',(0.744000000195517,-0.248000000195115,0.583389912844004));
#16893=CARTESIAN_POINT('Origin',(0.744000000194874,-0.744000000195115,0.583389912842708));
#16894=CARTESIAN_POINT('',(1.09999999999998,-0.248000000195576,1.19999999999984));
#16895=CARTESIAN_POINT('Origin',(1.10000000000007,-0.248000000195576,1.2));
#16896=CARTESIAN_POINT('',(0.744000000195517,-0.248000000195115,1.15122809938326));
#16897=CARTESIAN_POINT('Origin',(-3.14351440352569E-13,-0.24800000019415,
-5.12965591734105));
#16898=CARTESIAN_POINT('',(0.744000000195517,-0.248000000195115,1.2));
#16899=CARTESIAN_POINT('Origin',(-0.744000000195415,-0.744000000194864,
1.2));
#16900=CARTESIAN_POINT('',(-0.248000000195415,-0.744000000196249,1.15122809938316));
#16901=CARTESIAN_POINT('',(-0.744000000196312,-0.248000000194864,1.15122809938318));
#16902=CARTESIAN_POINT('Ctrl Pts',(-0.248000000195415,-0.744000000196249,
1.15122809938316));
#16903=CARTESIAN_POINT('Ctrl Pts',(-0.248000000195414,-0.74354812919633,
1.15128162561023));
#16904=CARTESIAN_POINT('Ctrl Pts',(-0.248000617699598,-0.743096462400134,
1.15133505381792));
#16905=CARTESIAN_POINT('Ctrl Pts',(-0.248170686680046,-0.680842516168463,
1.15868899091381));
#16906=CARTESIAN_POINT('Ctrl Pts',(-0.260619583353321,-0.614748859331044,
1.16502989619585));
#16907=CARTESIAN_POINT('Ctrl Pts',(-0.311166686725766,-0.49296651030398,
1.17344391775673));
#16908=CARTESIAN_POINT('Ctrl Pts',(-0.349270066586879,-0.437280006866388,
1.17551763482276));
#16909=CARTESIAN_POINT('Ctrl Pts',(-0.393275036726715,-0.393275036726509,
1.17551763482276));
#16910=CARTESIAN_POINT('Ctrl Pts',(-0.437280006866551,-0.349270066586629,
1.17551763482276));
#16911=CARTESIAN_POINT('Ctrl Pts',(-0.492966510304106,-0.311166686725461,
1.17344391775673));
#16912=CARTESIAN_POINT('Ctrl Pts',(-0.61474885933112,-0.260619583352896,
1.16502989619586));
#16913=CARTESIAN_POINT('Ctrl Pts',(-0.680842516168527,-0.248170686679557,
1.15868899091382));
#16914=CARTESIAN_POINT('Ctrl Pts',(-0.743096462400073,-0.248000617699049,
1.15133505381795));
#16915=CARTESIAN_POINT('Ctrl Pts',(-0.74354812919627,-0.248000000194863,
1.15128162561025));
#16916=CARTESIAN_POINT('Ctrl Pts',(-0.744000000196312,-0.248000000194864,
1.15122809938318));
#16917=CARTESIAN_POINT('',(-0.248000000195415,-0.744000000196249,0.58338991284606));
#16918=CARTESIAN_POINT('',(-0.248000000195415,-0.744000000196249,1.2));
#16919=CARTESIAN_POINT('',(-0.303056928861281,-0.516876228118006,0.19));
#16920=CARTESIAN_POINT('Origin',(-0.744000000195415,-0.744000000194864,
0.583389912845007));
#16921=CARTESIAN_POINT('',(-0.516876228118667,-0.303056928860673,0.19));
#16922=CARTESIAN_POINT('Origin',(-0.744000000195415,-0.744000000194864,
0.19));
#16923=CARTESIAN_POINT('',(-0.744000000196312,-0.248000000194864,0.583389912845176));
#16924=CARTESIAN_POINT('Origin',(-0.744000000195415,-0.744000000194864,
0.583389912843621));
#16925=CARTESIAN_POINT('',(-0.744000000196312,-0.248000000194864,1.2));
#16926=CARTESIAN_POINT('Origin',(-0.24800000019403,-0.248000000193966,1.2));
#16927=CARTESIAN_POINT('',(-1.04682989872298,-0.248000000195412,1.10790668314428));
#16928=CARTESIAN_POINT('Origin',(4.5589868649524E-13,-0.248000000193518,
-5.12965591734105));
#16929=CARTESIAN_POINT('',(-0.993500000024419,-0.248000000195315,1.01553658903588));
#16930=CARTESIAN_POINT('Origin',(0.744000000194874,-0.744000000195115,1.2));
#16931=CARTESIAN_POINT('',(0.248000000194874,-0.744000000196067,1.15122809938321));
#16932=CARTESIAN_POINT('Ctrl Pts',(0.744000000195517,-0.248000000195115,
1.15122809938326));
#16933=CARTESIAN_POINT('Ctrl Pts',(0.743548129195714,-0.248000000195114,
1.15128162561031));
#16934=CARTESIAN_POINT('Ctrl Pts',(0.743096462399633,-0.248000617699299,
1.15133505381799));
#16935=CARTESIAN_POINT('Ctrl Pts',(0.680842516168076,-0.248170686679796,
1.15868899091386));
#16936=CARTESIAN_POINT('Ctrl Pts',(0.614748859330666,-0.260619583353124,
1.1650298961959));
#16937=CARTESIAN_POINT('Ctrl Pts',(0.492966510303643,-0.311166686725667,
1.17344391775676));
#16938=CARTESIAN_POINT('Ctrl Pts',(0.437280006866081,-0.349270066586825,
1.17551763482279));
#16939=CARTESIAN_POINT('Ctrl Pts',(0.393275036726237,-0.393275036726696,
1.17551763482278));
#16940=CARTESIAN_POINT('Ctrl Pts',(0.349270066586393,-0.437280006866568,
1.17551763482278));
#16941=CARTESIAN_POINT('Ctrl Pts',(0.31116668672527,-0.492966510304154,
1.17344391775674));
#16942=CARTESIAN_POINT('Ctrl Pts',(0.260619583352803,-0.614748859331208,
1.16502989619586));
#16943=CARTESIAN_POINT('Ctrl Pts',(0.248170686679517,-0.680842516168625,
1.15868899091381));
#16944=CARTESIAN_POINT('Ctrl Pts',(0.248000617699059,-0.743096462400057,
1.15133505381795));
#16945=CARTESIAN_POINT('Ctrl Pts',(0.248000000194873,-0.743548129196139,
1.15128162561027));
#16946=CARTESIAN_POINT('Ctrl Pts',(0.248000000194874,-0.744000000196067,
1.15122809938321));
#16947=CARTESIAN_POINT('',(0.30305692886038,-0.516876228118955,0.19));
#16948=CARTESIAN_POINT('Origin',(0.744000000194874,-0.744000000195115,0.19));
#16949=CARTESIAN_POINT('',(0.248000000194874,-0.744000000196067,0.5833899128444));
#16950=CARTESIAN_POINT('Origin',(0.744000000194874,-0.744000000195115,0.583389912841405));
#16951=CARTESIAN_POINT('',(0.248000000194874,-0.744000000196067,1.2));
#16952=CARTESIAN_POINT('Origin',(0.248000000193922,-0.248000000194471,1.2));
#16953=CARTESIAN_POINT('',(0.248000000195456,-1.04682989872316,1.10790668314425));
#16954=CARTESIAN_POINT('Origin',(0.248000000193446,4.75999652275667E-13,
-5.12965591734105));
#16955=CARTESIAN_POINT('',(0.248000000195353,-0.993500000024651,1.01553658903593));
#16956=CARTESIAN_POINT('Origin',(-1.10000000000019,0.248000000196221,1.2));
#16957=CARTESIAN_POINT('',(-1.04682989872296,0.248000000196221,1.10790668314426));
#16958=CARTESIAN_POINT('Origin',(7.17605422133295E-15,0.248000000196221,
-5.12965591734105));
#16959=CARTESIAN_POINT('',(-1.10000000000019,0.248000000196221,1.2));
#16960=CARTESIAN_POINT('Origin',(-1.10000000000019,-0.248000000195508,1.2));
#16961=CARTESIAN_POINT('',(-1.04942373620595,-1.28517341949389E-16,1.11239934145138));
#16962=CARTESIAN_POINT('Origin',(1.91582141081578,-5.36035544273609E-16,
-4.02355591008731));
#16963=CARTESIAN_POINT('',(-0.516876228118667,-0.124000000097755,0.19));
#16964=CARTESIAN_POINT('Origin',(1.91582141081578,-5.36035544273609E-16,
-4.02355591008731));
#16965=CARTESIAN_POINT('Origin',(-0.248000000196409,-1.09999999999961,1.2));
#16966=CARTESIAN_POINT('',(-0.24800000019626,-1.04682989872243,1.10790668314434));
#16967=CARTESIAN_POINT('Origin',(-0.248000000193338,6.92337424395539E-13,
-5.12965591734105));
#16968=CARTESIAN_POINT('',(-0.248000000196409,-1.09999999999954,1.19999999999987));
#16969=CARTESIAN_POINT('Origin',(0.248000000195558,-1.10000000000039,1.2));
#16970=CARTESIAN_POINT('Origin',(3.00794342650252E-12,1.91582141081592,
-4.02355591008723));
#16971=CARTESIAN_POINT('',(0.124000000097801,-0.516876228118675,0.19));
#16972=CARTESIAN_POINT('Origin',(-5.91193760612896E-14,-1.66533453693773E-15,
0.19));
#16973=CARTESIAN_POINT('Origin',(0.,0.,-0.1));
#16974=CARTESIAN_POINT('',(0.939230484541328,-1.15022560655515E-16,0.));
#16975=CARTESIAN_POINT('Origin',(0.,0.,0.));
#16976=CARTESIAN_POINT('',(0.839230484541328,-1.02776092664042E-16,-0.1));
#16977=CARTESIAN_POINT('Origin',(0.939230484541328,-1.15022560655515E-16,
-0.1));
#16978=CARTESIAN_POINT('Origin',(0.,0.,-0.1));
#16979=CARTESIAN_POINT('Origin',(-0.839230484541328,0.,-7.24797437703358E-18));
#16980=CARTESIAN_POINT('',(2.15,-2.63299061816681E-16,0.));
#16981=CARTESIAN_POINT('Origin',(0.,0.,0.));
#16982=CARTESIAN_POINT('Origin',(0.,0.,-0.0749999999999998));
#16983=CARTESIAN_POINT('',(0.839230484541328,-1.02776092664042E-16,-0.15));
#16984=CARTESIAN_POINT('Origin',(0.,0.,-0.15));
#16985=CARTESIAN_POINT('',(0.839230484541328,-1.02776092664042E-16,-0.0749999999999998));
#16986=CARTESIAN_POINT('Origin',(0.,0.,-0.45));
#16987=CARTESIAN_POINT('',(0.96675,-1.1839272930757E-16,-0.625909310648334));
#16988=CARTESIAN_POINT('Origin',(0.,0.,-0.625909310648334));
#16989=CARTESIAN_POINT('',(0.919615242270664,-1.12620386289389E-16,-0.45));
#16990=CARTESIAN_POINT('Origin',(0.,0.,-3.375));
#16991=CARTESIAN_POINT('',(0.96675,1.1839272930757E-16,-6.));
#16992=CARTESIAN_POINT('Origin',(0.,0.,-6.));
#16993=CARTESIAN_POINT('',(0.96675,-1.1839272930757E-16,-3.375));
#16994=CARTESIAN_POINT('Origin',(0.,0.,-6.));
#16995=CARTESIAN_POINT('Origin',(7.21644966006352E-15,0.,-5.12965591734105));
#16996=CARTESIAN_POINT('',(-2.07563463599418,0.,0.85));
#16997=CARTESIAN_POINT('Origin',(7.21644966006352E-15,0.,-5.12965591734105));
#16998=CARTESIAN_POINT('',(2.07563463599418,-2.54191931316966E-16,0.85));
#16999=CARTESIAN_POINT('Origin',(0.,0.,0.85));
#17000=CARTESIAN_POINT('Origin',(0.,0.,0.85));
#17001=CARTESIAN_POINT('Origin',(0.,0.,0.425));
#17002=CARTESIAN_POINT('',(2.11281731799709,-2.58745496566823E-16,0.425));
#17003=CARTESIAN_POINT('',(6.5,-6.43177298256785,25.1137904048062));
#17004=CARTESIAN_POINT('',(6.5,-6.43177298256785,25.1137904048062));
#17005=CARTESIAN_POINT('',(6.5,-6.43177298256785,25.1137904048062));
#17006=CARTESIAN_POINT('',(6.5,-6.43177298256785,25.1137904048062));
#17007=CARTESIAN_POINT('',(6.5,-6.43177298256785,25.1137904048062));
#17008=CARTESIAN_POINT('',(6.5,-6.43177298256785,25.1137904048062));
#17009=CARTESIAN_POINT('',(6.5,-6.43177298256785,25.1137904048062));
#17010=CARTESIAN_POINT('',(6.5,-6.43177298256785,25.1137904048062));
#17011=CARTESIAN_POINT('',(9.,18.516026075963,54.6621693790315));
#17012=CARTESIAN_POINT('',(9.,18.5780788294298,2.70328105774178));
#17013=CARTESIAN_POINT('',(9.,-12.4371726180826,2.70328105774178));
#17014=CARTESIAN_POINT('',(9.,-12.3751198646158,54.6621693790315));
#17015=UNCERTAINTY_MEASURE_WITH_UNIT(LENGTH_MEASURE(0.01),#17043,
'DISTANCE_ACCURACY_VALUE',
'Maximum model space distance between geometric entities at asserted c
onnectivities');
#17016=UNCERTAINTY_MEASURE_WITH_UNIT(LENGTH_MEASURE(0.01),#17043,
'DISTANCE_ACCURACY_VALUE',
'Maximum model space distance between geometric entities at asserted c
onnectivities');
#17017=UNCERTAINTY_MEASURE_WITH_UNIT(LENGTH_MEASURE(0.01),#17043,
'DISTANCE_ACCURACY_VALUE',
'Maximum model space distance between geometric entities at asserted c
onnectivities');
#17018=UNCERTAINTY_MEASURE_WITH_UNIT(LENGTH_MEASURE(0.01),#17043,
'DISTANCE_ACCURACY_VALUE',
'Maximum model space distance between geometric entities at asserted c
onnectivities');
#17019=UNCERTAINTY_MEASURE_WITH_UNIT(LENGTH_MEASURE(0.01),#17043,
'DISTANCE_ACCURACY_VALUE',
'Maximum model space distance between geometric entities at asserted c
onnectivities');
#17020=UNCERTAINTY_MEASURE_WITH_UNIT(LENGTH_MEASURE(0.01),#17043,
'DISTANCE_ACCURACY_VALUE',
'Maximum model space distance between geometric entities at asserted c
onnectivities');
#17021=UNCERTAINTY_MEASURE_WITH_UNIT(LENGTH_MEASURE(0.01),#17043,
'DISTANCE_ACCURACY_VALUE',
'Maximum model space distance between geometric entities at asserted c
onnectivities');
#17022=UNCERTAINTY_MEASURE_WITH_UNIT(LENGTH_MEASURE(0.01),#17043,
'DISTANCE_ACCURACY_VALUE',
'Maximum model space distance between geometric entities at asserted c
onnectivities');
#17023=UNCERTAINTY_MEASURE_WITH_UNIT(LENGTH_MEASURE(0.01),#17043,
'DISTANCE_ACCURACY_VALUE',
'Maximum model space distance between geometric entities at asserted c
onnectivities');
#17024=UNCERTAINTY_MEASURE_WITH_UNIT(LENGTH_MEASURE(0.01),#17043,
'DISTANCE_ACCURACY_VALUE',
'Maximum model space distance between geometric entities at asserted c
onnectivities');
#17025=UNCERTAINTY_MEASURE_WITH_UNIT(LENGTH_MEASURE(0.01),#17043,
'DISTANCE_ACCURACY_VALUE',
'Maximum model space distance between geometric entities at asserted c
onnectivities');
#17026=UNCERTAINTY_MEASURE_WITH_UNIT(LENGTH_MEASURE(0.01),#17043,
'DISTANCE_ACCURACY_VALUE',
'Maximum model space distance between geometric entities at asserted c
onnectivities');
#17027=UNCERTAINTY_MEASURE_WITH_UNIT(LENGTH_MEASURE(0.01),#17043,
'DISTANCE_ACCURACY_VALUE',
'Maximum model space distance between geometric entities at asserted c
onnectivities');
#17028=UNCERTAINTY_MEASURE_WITH_UNIT(LENGTH_MEASURE(0.01),#17043,
'DISTANCE_ACCURACY_VALUE',
'Maximum model space distance between geometric entities at asserted c
onnectivities');
#17029=(
GEOMETRIC_REPRESENTATION_CONTEXT(3)
GLOBAL_UNCERTAINTY_ASSIGNED_CONTEXT((#17015))
GLOBAL_UNIT_ASSIGNED_CONTEXT((#17043,#17045,#17046))
REPRESENTATION_CONTEXT('','3D')
);
#17030=(
GEOMETRIC_REPRESENTATION_CONTEXT(3)
GLOBAL_UNCERTAINTY_ASSIGNED_CONTEXT((#17016))
GLOBAL_UNIT_ASSIGNED_CONTEXT((#17043,#17045,#17046))
REPRESENTATION_CONTEXT('','3D')
);
#17031=(
GEOMETRIC_REPRESENTATION_CONTEXT(3)
GLOBAL_UNCERTAINTY_ASSIGNED_CONTEXT((#17017))
GLOBAL_UNIT_ASSIGNED_CONTEXT((#17043,#17045,#17046))
REPRESENTATION_CONTEXT('','3D')
);
#17032=(
GEOMETRIC_REPRESENTATION_CONTEXT(3)
GLOBAL_UNCERTAINTY_ASSIGNED_CONTEXT((#17018))
GLOBAL_UNIT_ASSIGNED_CONTEXT((#17043,#17045,#17046))
REPRESENTATION_CONTEXT('','3D')
);
#17033=(
GEOMETRIC_REPRESENTATION_CONTEXT(3)
GLOBAL_UNCERTAINTY_ASSIGNED_CONTEXT((#17019))
GLOBAL_UNIT_ASSIGNED_CONTEXT((#17043,#17045,#17046))
REPRESENTATION_CONTEXT('','3D')
);
#17034=(
GEOMETRIC_REPRESENTATION_CONTEXT(3)
GLOBAL_UNCERTAINTY_ASSIGNED_CONTEXT((#17020))
GLOBAL_UNIT_ASSIGNED_CONTEXT((#17043,#17045,#17046))
REPRESENTATION_CONTEXT('','3D')
);
#17035=(
GEOMETRIC_REPRESENTATION_CONTEXT(3)
GLOBAL_UNCERTAINTY_ASSIGNED_CONTEXT((#17021))
GLOBAL_UNIT_ASSIGNED_CONTEXT((#17043,#17045,#17046))
REPRESENTATION_CONTEXT('','3D')
);
#17036=(
GEOMETRIC_REPRESENTATION_CONTEXT(3)
GLOBAL_UNCERTAINTY_ASSIGNED_CONTEXT((#17022))
GLOBAL_UNIT_ASSIGNED_CONTEXT((#17043,#17045,#17046))
REPRESENTATION_CONTEXT('','3D')
);
#17037=(
GEOMETRIC_REPRESENTATION_CONTEXT(3)
GLOBAL_UNCERTAINTY_ASSIGNED_CONTEXT((#17023))
GLOBAL_UNIT_ASSIGNED_CONTEXT((#17043,#17045,#17046))
REPRESENTATION_CONTEXT('','3D')
);
#17038=(
GEOMETRIC_REPRESENTATION_CONTEXT(3)
GLOBAL_UNCERTAINTY_ASSIGNED_CONTEXT((#17024))
GLOBAL_UNIT_ASSIGNED_CONTEXT((#17043,#17045,#17046))
REPRESENTATION_CONTEXT('','3D')
);
#17039=(
GEOMETRIC_REPRESENTATION_CONTEXT(3)
GLOBAL_UNCERTAINTY_ASSIGNED_CONTEXT((#17025))
GLOBAL_UNIT_ASSIGNED_CONTEXT((#17043,#17045,#17046))
REPRESENTATION_CONTEXT('','3D')
);
#17040=(
GEOMETRIC_REPRESENTATION_CONTEXT(3)
GLOBAL_UNCERTAINTY_ASSIGNED_CONTEXT((#17026))
GLOBAL_UNIT_ASSIGNED_CONTEXT((#17043,#17045,#17046))
REPRESENTATION_CONTEXT('','3D')
);
#17041=(
GEOMETRIC_REPRESENTATION_CONTEXT(3)
GLOBAL_UNCERTAINTY_ASSIGNED_CONTEXT((#17027))
GLOBAL_UNIT_ASSIGNED_CONTEXT((#17043,#17045,#17046))
REPRESENTATION_CONTEXT('','3D')
);
#17042=(
GEOMETRIC_REPRESENTATION_CONTEXT(3)
GLOBAL_UNCERTAINTY_ASSIGNED_CONTEXT((#17028))
GLOBAL_UNIT_ASSIGNED_CONTEXT((#17043,#17045,#17046))
REPRESENTATION_CONTEXT('','3D')
);
#17043=(
LENGTH_UNIT()
NAMED_UNIT(*)
SI_UNIT(.MILLI.,.METRE.)
);
#17044=(
LENGTH_UNIT()
NAMED_UNIT(*)
SI_UNIT($,.METRE.)
);
#17045=(
NAMED_UNIT(*)
PLANE_ANGLE_UNIT()
SI_UNIT($,.RADIAN.)
);
#17046=(
NAMED_UNIT(*)
SI_UNIT($,.STERADIAN.)
SOLID_ANGLE_UNIT()
);
#17047=SHAPE_DEFINITION_REPRESENTATION(#17060,#17085);
#17048=SHAPE_DEFINITION_REPRESENTATION(#17061,#17086);
#17049=SHAPE_DEFINITION_REPRESENTATION(#17062,#17087);
#17050=SHAPE_DEFINITION_REPRESENTATION(#17063,#17088);
#17051=SHAPE_DEFINITION_REPRESENTATION(#17064,#17089);
#17052=SHAPE_DEFINITION_REPRESENTATION(#17065,#17090);
#17053=SHAPE_DEFINITION_REPRESENTATION(#17066,#17091);
#17054=SHAPE_DEFINITION_REPRESENTATION(#17067,#17092);
#17055=SHAPE_DEFINITION_REPRESENTATION(#17068,#17093);
#17056=SHAPE_DEFINITION_REPRESENTATION(#17069,#17094);
#17057=SHAPE_DEFINITION_REPRESENTATION(#17070,#17095);
#17058=SHAPE_DEFINITION_REPRESENTATION(#17071,#17096);
#17059=SHAPE_DEFINITION_REPRESENTATION(#17072,#17097);
#17060=PRODUCT_DEFINITION_SHAPE('',$,#17099);
#17061=PRODUCT_DEFINITION_SHAPE('',$,#17100);
#17062=PRODUCT_DEFINITION_SHAPE('',$,#17101);
#17063=PRODUCT_DEFINITION_SHAPE('',$,#17102);
#17064=PRODUCT_DEFINITION_SHAPE('',$,#17103);
#17065=PRODUCT_DEFINITION_SHAPE('',$,#17104);
#17066=PRODUCT_DEFINITION_SHAPE('',$,#17105);
#17067=PRODUCT_DEFINITION_SHAPE('',$,#17106);
#17068=PRODUCT_DEFINITION_SHAPE('',$,#17107);
#17069=PRODUCT_DEFINITION_SHAPE('',$,#17108);
#17070=PRODUCT_DEFINITION_SHAPE('',$,#17109);
#17071=PRODUCT_DEFINITION_SHAPE('',$,#17110);
#17072=PRODUCT_DEFINITION_SHAPE('',$,#17111);
#17073=PRODUCT_DEFINITION_SHAPE($,$,#47);
#17074=PRODUCT_DEFINITION_SHAPE($,$,#48);
#17075=PRODUCT_DEFINITION_SHAPE($,$,#49);
#17076=PRODUCT_DEFINITION_SHAPE($,$,#50);
#17077=PRODUCT_DEFINITION_SHAPE($,$,#51);
#17078=PRODUCT_DEFINITION_SHAPE($,$,#52);
#17079=PRODUCT_DEFINITION_SHAPE($,$,#53);
#17080=PRODUCT_DEFINITION_SHAPE($,$,#54);
#17081=PRODUCT_DEFINITION_SHAPE($,$,#55);
#17082=PRODUCT_DEFINITION_SHAPE($,$,#56);
#17083=PRODUCT_DEFINITION_SHAPE($,$,#57);
#17084=PRODUCT_DEFINITION_SHAPE($,$,#58);
#17085=SHAPE_REPRESENTATION('',(#8260,#9239,#9240,#9241,#9242,#9243,#9244,
#9245,#9246,#9247,#9248,#9249,#9250),#17029);
#17086=SHAPE_REPRESENTATION('',(#8261),#17030);
#17087=SHAPE_REPRESENTATION('',(#8462),#17031);
#17088=SHAPE_REPRESENTATION('',(#8601),#17032);
#17089=SHAPE_REPRESENTATION('',(#8648),#17033);
#17090=SHAPE_REPRESENTATION('',(#8826),#17034);
#17091=SHAPE_REPRESENTATION('',(#8839),#17035);
#17092=SHAPE_REPRESENTATION('',(#8908),#17036);
#17093=SHAPE_REPRESENTATION('',(#8935),#17037);
#17094=SHAPE_REPRESENTATION('',(#8995),#17038);
#17095=SHAPE_REPRESENTATION('',(#9056),#17039);
#17096=SHAPE_REPRESENTATION('',(#9117),#17040);
#17097=SHAPE_REPRESENTATION('',(#9178),#17041);
#17098=PRODUCT_DEFINITION_CONTEXT('part definition',#17139,'design');
#17099=PRODUCT_DEFINITION('MAS-262','MAS-262',#17112,#17098);
#17100=PRODUCT_DEFINITION('CLAMSHELL_TOP','CLAMSHELL_TOP',#17113,#17098);
#17101=PRODUCT_DEFINITION('CLAMSHELL_BOT','CLAMSHELL_BOT',#17114,#17098);
#17102=PRODUCT_DEFINITION('EXTENSION_100MM','EXTENSION_100MM',#17115,#17098);
#17103=PRODUCT_DEFINITION('GUIDE','GUIDE',#17116,#17098);
#17104=PRODUCT_DEFINITION('SHAFT_100MM','SHAFT_100MM',#17117,#17098);
#17105=PRODUCT_DEFINITION('PLUG','PLUG',#17118,#17098);
#17106=PRODUCT_DEFINITION('Nut','Nut',#17119,#17098);
#17107=PRODUCT_DEFINITION('GROMMET','GROMMET',#17120,#17098);
#17108=PRODUCT_DEFINITION('BHS JIS B 1111 - M2x6 Steel 4.6 Plain',
'Binding Head Screw JIS B 1111 - M2x6 Steel 4.6 Plain v1',#17121,#17098);
#17109=PRODUCT_DEFINITION('BHS JIS B 1111 - M2x6 Steel 4.6 Plain_1',
'Binding Head Screw JIS B 1111 - M2x6 Steel 4.6 Plain v1 (2)',#17122,#17098);
#17110=PRODUCT_DEFINITION('BHS JIS B 1111 - M2x6 Steel 4.6 Plain_2',
'Binding Head Screw JIS B 1111 - M2x6 Steel 4.6 Plain v1 (3)',#17123,#17098);
#17111=PRODUCT_DEFINITION('BHS JIS B 1111 - M2x6 Steel 4.6 Plain_3',
'Binding Head Screw JIS B 1111 - M2x6 Steel 4.6 Plain v1 (1)',#17124,#17098);
#17112=PRODUCT_DEFINITION_FORMATION('',$,#17141);
#17113=PRODUCT_DEFINITION_FORMATION('',$,#17142);
#17114=PRODUCT_DEFINITION_FORMATION('',$,#17143);
#17115=PRODUCT_DEFINITION_FORMATION('',$,#17144);
#17116=PRODUCT_DEFINITION_FORMATION('',$,#17145);
#17117=PRODUCT_DEFINITION_FORMATION('',$,#17146);
#17118=PRODUCT_DEFINITION_FORMATION('',$,#17147);
#17119=PRODUCT_DEFINITION_FORMATION('',$,#17148);
#17120=PRODUCT_DEFINITION_FORMATION('',$,#17149);
#17121=PRODUCT_DEFINITION_FORMATION('',$,#17150);
#17122=PRODUCT_DEFINITION_FORMATION('',$,#17151);
#17123=PRODUCT_DEFINITION_FORMATION('',$,#17152);
#17124=PRODUCT_DEFINITION_FORMATION('',$,#17153);
#17125=PRODUCT_RELATED_PRODUCT_CATEGORY('MAS-262','MAS-262',(#17141));
#17126=PRODUCT_RELATED_PRODUCT_CATEGORY('CLAMSHELL_TOP','CLAMSHELL_TOP',
(#17142));
#17127=PRODUCT_RELATED_PRODUCT_CATEGORY('CLAMSHELL_BOT','CLAMSHELL_BOT',
(#17143));
#17128=PRODUCT_RELATED_PRODUCT_CATEGORY('EXTENSION_100MM',
'EXTENSION_100MM',(#17144));
#17129=PRODUCT_RELATED_PRODUCT_CATEGORY('GUIDE','GUIDE',(#17145));
#17130=PRODUCT_RELATED_PRODUCT_CATEGORY('SHAFT_100MM','SHAFT_100MM',(#17146));
#17131=PRODUCT_RELATED_PRODUCT_CATEGORY('PLUG','PLUG',(#17147));
#17132=PRODUCT_RELATED_PRODUCT_CATEGORY('Nut','Nut',(#17148));
#17133=PRODUCT_RELATED_PRODUCT_CATEGORY('GROMMET','GROMMET',(#17149));
#17134=PRODUCT_RELATED_PRODUCT_CATEGORY(
'Binding Head Screw JIS B 1111 - M2x6 Steel 4.6 Plain v1',
'Binding Head Screw JIS B 1111 - M2x6 Steel 4.6 Plain v1',(#17150));
#17135=PRODUCT_RELATED_PRODUCT_CATEGORY(
'Binding Head Screw JIS B 1111 - M2x6 Steel 4.6 Plain v1 (2)',
'Binding Head Screw JIS B 1111 - M2x6 Steel 4.6 Plain v1 (2)',(#17151));
#17136=PRODUCT_RELATED_PRODUCT_CATEGORY(
'Binding Head Screw JIS B 1111 - M2x6 Steel 4.6 Plain v1 (3)',
'Binding Head Screw JIS B 1111 - M2x6 Steel 4.6 Plain v1 (3)',(#17152));
#17137=PRODUCT_RELATED_PRODUCT_CATEGORY(
'Binding Head Screw JIS B 1111 - M2x6 Steel 4.6 Plain v1 (1)',
'Binding Head Screw JIS B 1111 - M2x6 Steel 4.6 Plain v1 (1)',(#17153));
#17138=APPLICATION_PROTOCOL_DEFINITION('international standard',
'automotive_design',2009,#17139);
#17139=APPLICATION_CONTEXT(
'Core Data for Automotive Mechanical Design Process');
#17140=PRODUCT_CONTEXT('part definition',#17139,'mechanical');
#17141=PRODUCT('MAS-262','MAS-262',$,(#17140));
#17142=PRODUCT('CLAMSHELL_TOP','CLAMSHELL_TOP',$,(#17140));
#17143=PRODUCT('CLAMSHELL_BOT','CLAMSHELL_BOT',$,(#17140));
#17144=PRODUCT('EXTENSION_100MM','EXTENSION_100MM',$,(#17140));
#17145=PRODUCT('GUIDE','GUIDE',$,(#17140));
#17146=PRODUCT('SHAFT_100MM','SHAFT_100MM',$,(#17140));
#17147=PRODUCT('PLUG','PLUG',$,(#17140));
#17148=PRODUCT('Nut','Nut',$,(#17140));
#17149=PRODUCT('GROMMET','GROMMET',$,(#17140));
#17150=PRODUCT('BHS JIS B 1111 - M2x6 Steel 4.6 Plain',
'Binding Head Screw JIS B 1111 - M2x6 Steel 4.6 Plain v1',
'Binding Head Screw JIS B 1111 - M2x6',(#17140));
#17151=PRODUCT('BHS JIS B 1111 - M2x6 Steel 4.6 Plain_1',
'Binding Head Screw JIS B 1111 - M2x6 Steel 4.6 Plain v1 (2)',
'Binding Head Screw JIS B 1111 - M2x6',(#17140));
#17152=PRODUCT('BHS JIS B 1111 - M2x6 Steel 4.6 Plain_2',
'Binding Head Screw JIS B 1111 - M2x6 Steel 4.6 Plain v1 (3)',
'Binding Head Screw JIS B 1111 - M2x6',(#17140));
#17153=PRODUCT('BHS JIS B 1111 - M2x6 Steel 4.6 Plain_3',
'Binding Head Screw JIS B 1111 - M2x6 Steel 4.6 Plain v1 (1)',
'Binding Head Screw JIS B 1111 - M2x6',(#17140));
#17154=PRESENTATION_STYLE_ASSIGNMENT((#17155));
#17155=SURFACE_STYLE_USAGE(.BOTH.,#17156);
#17156=SURFACE_SIDE_STYLE('',(#17157));
#17157=SURFACE_STYLE_FILL_AREA(#17158);
#17158=FILL_AREA_STYLE('Steel - Satin',(#17159));
#17159=FILL_AREA_STYLE_COLOUR('Steel - Satin',#17160);
#17160=COLOUR_RGB('Steel - Satin', 0.09019608, 0.27058824, 0.51372549);
ENDSEC;
END-ISO-10303-21;
